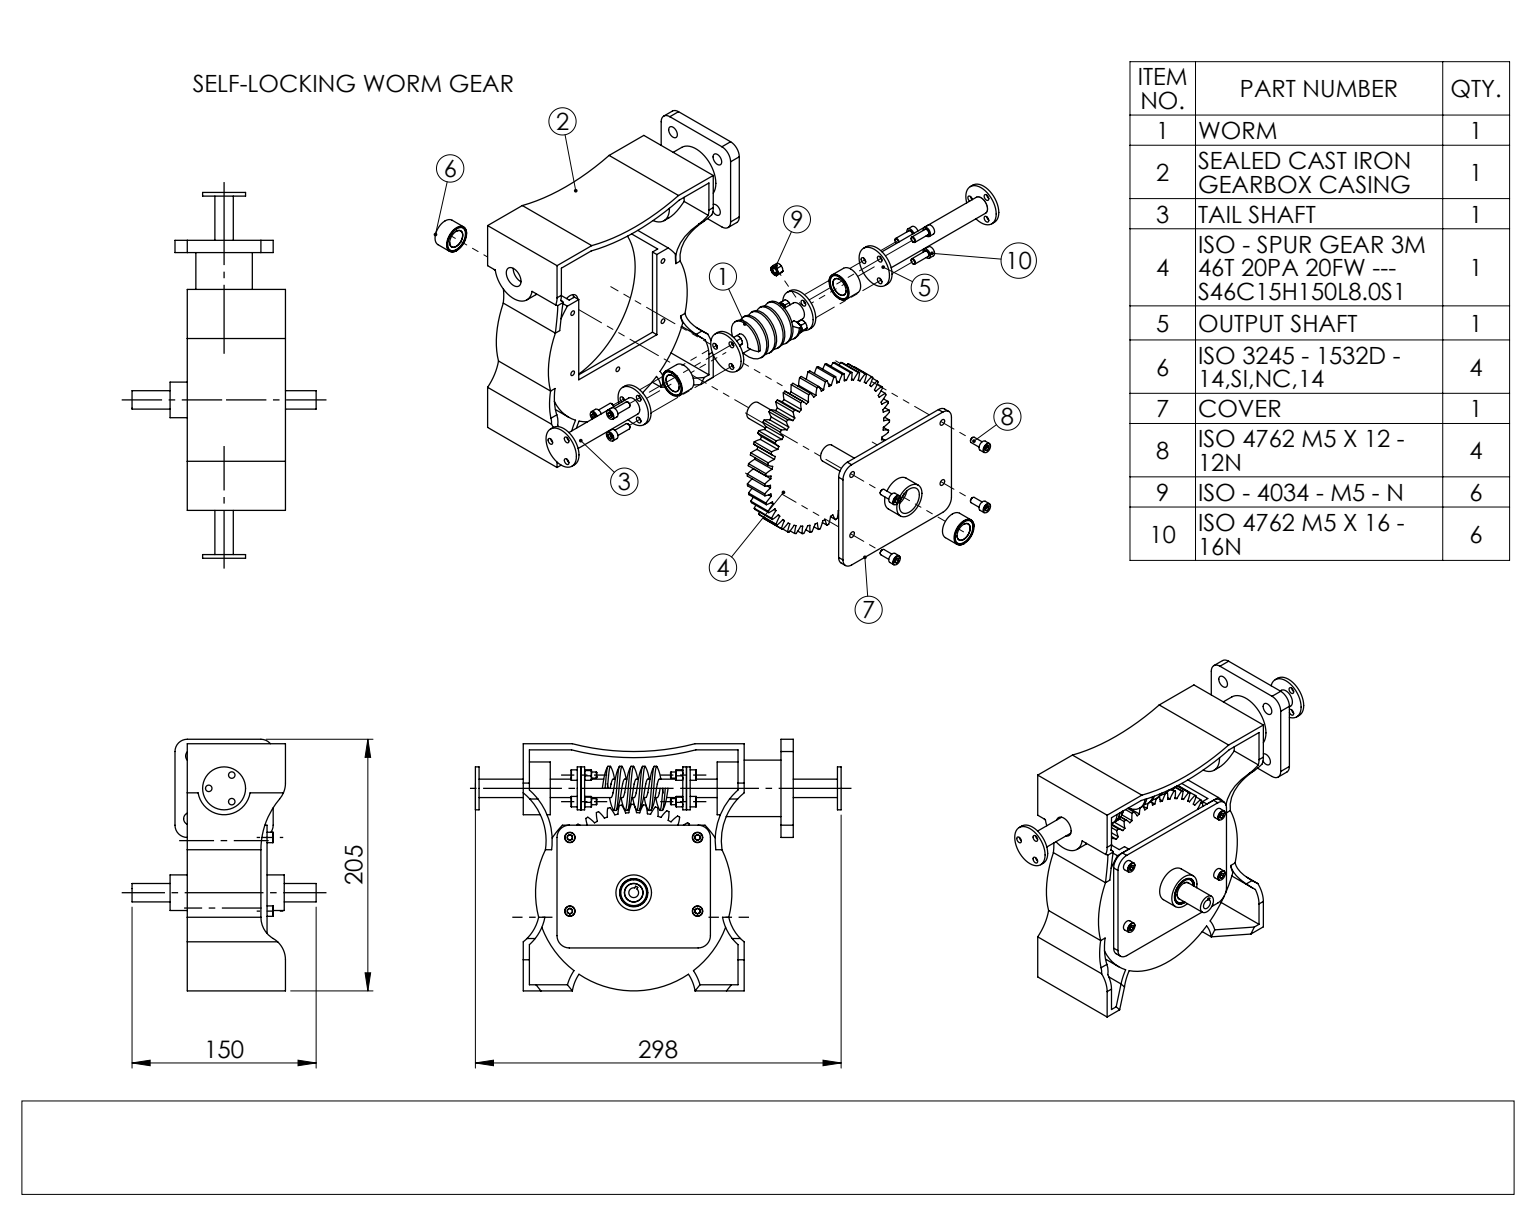
ISO-10303-21;
HEADER;
FILE_DESCRIPTION (('STEP AP214'),
    '1' );
FILE_NAME ('BR-546',
    '2026-10-03T12:29:21',
    ( '' ),
    ( '' ),
    'SwSTEP 2.0',
    'SolidWorks 2026',
    '' );
FILE_SCHEMA (( 'AUTOMOTIVE_DESIGN' ));
ENDSEC;

DATA;
#1 = CARTESIAN_POINT ( 'NONE',  ( 19.99999999999999645, 0.000000000000000000, 0.000000000000000000 ) ) ;
#2 = CARTESIAN_POINT ( 'NONE',  ( -6.358192987158596488, 4.248408730893249441, 12.23479375018031590 ) ) ;
#3 = ADVANCED_FACE ( 'NONE', ( #6649 ), #1884, .F. ) ;
#4 = CARTESIAN_POINT ( 'NONE',  ( 11.17563879758427525, 2.222972768810836719, -0.3496410002868030609 ) ) ;
#5 = ADVANCED_FACE ( 'NONE', ( #12919 ), #11518, .F. ) ;
#6 = DIRECTION ( 'NONE',  ( 0.000000000000000000, 0.000000000000000000, -1.000000000000000000 ) ) ;
#7 = CARTESIAN_POINT ( 'NONE',  ( -30.00000000000000000, -42.57363661491096707, -71.38288848018790134 ) ) ;
#8 = DIRECTION ( 'NONE',  ( 0.000000000000000000, 0.000000000000000000, 1.000000000000000000 ) ) ;
#9 = ORIENTED_EDGE ( 'NONE', *, *, #5715, .F. ) ;
#10 = CYLINDRICAL_SURFACE ( 'NONE', #420, 72.00000000007199219 ) ;
#11 = VERTEX_POINT ( 'NONE', #11628 ) ;
#12 = AXIS2_PLACEMENT_3D ( 'NONE', #6697, #8706, #19835 ) ;
#13 = CARTESIAN_POINT ( 'NONE',  ( 16.62983158437509346, -6.888301784570739272, 14.47261250018031298 ) ) ;
#14 = DIRECTION ( 'NONE',  ( -1.000000000000000000, 0.000000000000000000, 0.000000000000000000 ) ) ;
#15 = ADVANCED_FACE ( 'NONE', ( #19478 ), #14650, .T. ) ;
#16 = ORIENTED_EDGE ( 'NONE', *, *, #12265, .T. ) ;
#17 = CARTESIAN_POINT ( 'NONE',  ( 24.99999999999999645, -39.99999999999999289, 52.00000000000000000 ) ) ;
#18 = EDGE_LOOP ( 'NONE', ( #17253, #7628, #12680, #16637 ) ) ;
#19 = DIRECTION ( 'NONE',  ( -1.000000000000000000, 0.000000000000000000, -0.000000000000000000 ) ) ;
#20 = CARTESIAN_POINT ( 'NONE',  ( 33.05469362121638000, -30.48475803102838100, 72.85691518208254536 ) ) ;
#21 = ORIENTED_EDGE ( 'NONE', *, *, #4326, .F. ) ;
#22 =( GEOMETRIC_REPRESENTATION_CONTEXT ( 3 ) GLOBAL_UNCERTAINTY_ASSIGNED_CONTEXT ( ( #13875 ) ) GLOBAL_UNIT_ASSIGNED_CONTEXT ( ( #2142, #14970, #8601 ) ) REPRESENTATION_CONTEXT ( 'NONE', 'WORKASPACE' ) );
#23 = ORIENTED_EDGE ( 'NONE', *, *, #11876, .F. ) ;
#24 = DIRECTION ( 'NONE',  ( -1.000000000000000000, -0.000000000000000000, 0.000000000000000000 ) ) ;
#25 = CARTESIAN_POINT ( 'NONE',  ( 19.99999999999999645, 0.000000000000000000, 0.000000000000000000 ) ) ;
#26 = EDGE_CURVE ( 'NONE', #19472, #5238, #10237, .T. ) ;
#27 = AXIS2_PLACEMENT_3D ( 'NONE', #16790, #15301, #10014 ) ;
#28 = CARTESIAN_POINT ( 'NONE',  ( -30.00000000000000000, -85.00000000000000000, -1.040949779275250179E-14 ) ) ;
#29 = ORIENTED_EDGE ( 'NONE', *, *, #16424, .T. ) ;
#30 = ADVANCED_FACE ( 'NONE', ( #14609 ), #17902, .T. ) ;
#31 = CARTESIAN_POINT ( 'NONE',  ( -6.358192987158591158, 4.248408730893245000, 5.969893750180312431 ) ) ;
#32 = VECTOR ( 'NONE', #14335, 1000.000000000000000 ) ;
#33 = EDGE_CURVE ( 'NONE', #6658, #4014, #18101, .T. ) ;
#34 = CARTESIAN_POINT ( 'NONE',  ( 6.358192987158596488, -4.248408730893249441, -1.902706249819686279 ) ) ;
#35 = AXIS2_PLACEMENT_3D ( 'NONE', #14775, #17865, #16462 ) ;
#36 = CARTESIAN_POINT ( 'NONE',  ( 0.000000000000000000, 0.000000000000000000, 40.00000000000000000 ) ) ;
#37 = DIRECTION ( 'NONE',  ( 0.000000000000000000, 0.000000000000000000, -1.000000000000000000 ) ) ;
#38 = EDGE_CURVE ( 'NONE', #16141, #4659, #188, .T. ) ;
#39 = ORIENTED_EDGE ( 'NONE', *, *, #4985, .T. ) ;
#40 = DIRECTION ( 'NONE',  ( -0.000000000000000000, -0.000000000000000000, -1.000000000000000000 ) ) ;
#41 = CARTESIAN_POINT ( 'NONE',  ( -6.165580000000000283, 0.000000000000000000, 0.000000000000000000 ) ) ;
#42 = ORIENTED_EDGE ( 'NONE', *, *, #280, .F. ) ;
#43 = PLANE ( 'NONE',  #3162 ) ;
#44 = VERTEX_POINT ( 'NONE', #17992 ) ;
#45 = CARTESIAN_POINT ( 'NONE',  ( 19.99999999999999645, -20.60847369612940128, -61.90898814327737654 ) ) ;
#46 = ORIENTED_EDGE ( 'NONE', *, *, #5820, .T. ) ;
#47 = VECTOR ( 'NONE', #20298, 1000.000000000000000 ) ;
#48 = DIRECTION ( 'NONE',  ( 0.000000000000000000, 0.000000000000000000, -1.000000000000000000 ) ) ;
#49 = EDGE_CURVE ( 'NONE', #12259, #9717, #8442, .T. ) ;
#50 = DIRECTION ( 'NONE',  ( 0.000000000000000000, 0.000000000000000000, -1.000000000000000000 ) ) ;
#51 = CIRCLE ( 'NONE', #6813, 3.199999999999994404 ) ;
#52 = CARTESIAN_POINT ( 'NONE',  ( 14.79893867793684059, 2.943691925285398359, -12.82923933115845649 ) ) ;
#53 = ORIENTED_EDGE ( 'NONE', *, *, #13639, .F. ) ;
#54 = DIRECTION ( 'NONE',  ( 0.000000000000000000, -1.000000000000000000, 0.000000000000000000 ) ) ;
#55 = ADVANCED_FACE ( 'NONE', ( #11330 ), #295, .T. ) ;
#56 = DIRECTION ( 'NONE',  ( 0.000000000000000000, 0.000000000000000000, 1.000000000000000000 ) ) ;
#57 = EDGE_LOOP ( 'NONE', ( #4970, #17934 ) ) ;
#58 = CIRCLE ( 'NONE', #5129, 27.60000000002759890 ) ;
#59 = CARTESIAN_POINT ( 'NONE',  ( 40.00000000000000711, 29.99999999999999289, -120.0000000000000142 ) ) ;
#60 = VECTOR ( 'NONE', #20579, 1000.000000000000000 ) ;
#61 = CARTESIAN_POINT ( 'NONE',  ( -15.25966317163203279, -10.19618095047498052, 17.71245625018031689 ) ) ;
#62 = VECTOR ( 'NONE', #8354, 1000.000000000000000 ) ;
#63 = LINE ( 'NONE', #20325, #13108 ) ;
#64 = DIRECTION ( 'NONE',  ( 0.000000000000000000, 0.000000000000000000, 1.000000000000000000 ) ) ;
#65 = VERTEX_POINT ( 'NONE', #16100 ) ;
#66 = ADVANCED_FACE ( 'NONE', ( #13335 ), #6435, .F. ) ;
#67 = CARTESIAN_POINT ( 'NONE',  ( 0.000000000000000000, 0.000000000000000000, 0.000000000000000000 ) ) ;
#68 =( GEOMETRIC_REPRESENTATION_CONTEXT ( 3 ) GLOBAL_UNCERTAINTY_ASSIGNED_CONTEXT ( ( #15146 ) ) GLOBAL_UNIT_ASSIGNED_CONTEXT ( ( #18068, #7816, #19263 ) ) REPRESENTATION_CONTEXT ( 'NONE', 'WORKASPACE' ) );
#69 = ORIENTED_EDGE ( 'NONE', *, *, #783, .F. ) ;
#70 = CARTESIAN_POINT ( 'NONE',  ( 0.000000000000000000, 38.69327817041775575, 52.53819777490647880 ) ) ;
#71 = DIRECTION ( 'NONE',  ( 0.000000000000000000, 0.000000000000000000, 1.000000000000000000 ) ) ;
#72 = CARTESIAN_POINT ( 'NONE',  ( 1.491842756249030399, 7.499999999820669672, -4.848018749819687834 ) ) ;
#73 = ORIENTED_EDGE ( 'NONE', *, *, #769, .F. ) ;
#74 = DIRECTION ( 'NONE',  ( 0.000000000000000000, 0.4999999999999990008, -0.8660254037844391517 ) ) ;
#75 = AXIS2_PLACEMENT_3D ( 'NONE', #412, #6863, #13354 ) ;
#76 = AXIS2_PLACEMENT_3D ( 'NONE', #4116, #10601, #17063 ) ;
#77 = CARTESIAN_POINT ( 'NONE',  ( -7.500000000000000000, 0.000000000000000000, 126.0000000000000000 ) ) ;
#78 = TOROIDAL_SURFACE ( 'NONE', #2431, 2.700000000000000622, 0.2000000000000000111 ) ;
#79 = APPLICATION_PROTOCOL_DEFINITION ( 'draft international standard', 'automotive_design', 1998, #17252 ) ;
#80 = CARTESIAN_POINT ( 'NONE',  ( 3.580422614997669228, 17.99999999956958874, -7.028168749819693417 ) ) ;
#81 = ORIENTED_EDGE ( 'NONE', *, *, #16157, .T. ) ;
#82 = DIRECTION ( 'NONE',  ( 0.000000000000000000, -0.2697967711570314897, 0.9629172873477973571 ) ) ;
#83 = CARTESIAN_POINT ( 'NONE',  ( -13.67243654778935102, -5.663308646854334327, -4.604354418480926192 ) ) ;
#84 = DIRECTION ( 'NONE',  ( -1.000000000000000000, -0.000000000000000000, -0.000000000000000000 ) ) ;
#85 = VECTOR ( 'NONE', #11262, 1000.000000000000000 ) ;
#86 = ADVANCED_FACE ( 'NONE', ( #9826 ), #1783, .F. ) ;
#87 = ORIENTED_EDGE ( 'NONE', *, *, #13366, .F. ) ;
#88 = EDGE_CURVE ( 'NONE', #14573, #2530, #13132, .T. ) ;
#89 = DIRECTION ( 'NONE',  ( -1.000000000000000000, 0.000000000000000000, 0.000000000000000000 ) ) ;
#90 = DIRECTION ( 'NONE',  ( -0.000000000000000000, -0.000000000000000000, 1.000000000000000000 ) ) ;
#91 = CARTESIAN_POINT ( 'NONE',  ( 150.0000507999999968, 5.400000000000000355, 1.000000000000000000 ) ) ;
#92 = ORIENTED_EDGE ( 'NONE', *, *, #14677, .F. ) ;
#93 = DIRECTION ( 'NONE',  ( -0.000000000000000000, 0.000000000000000000, 1.000000000000000000 ) ) ;
#94 = ORIENTED_EDGE ( 'NONE', *, *, #11160, .T. ) ;
#95 = FACE_OUTER_BOUND ( 'NONE', #12969, .T. ) ;
#96 = CARTESIAN_POINT ( 'NONE',  ( 0.000000000000000000, -3.141410481200616278, -65.17333458706190186 ) ) ;
#97 = B_SPLINE_CURVE_WITH_KNOTS ( 'NONE', 3,
 ( #16276, #17575, #14698, #9503, #6729, #17780 ),
 .UNSPECIFIED., .F., .F.,
 ( 4, 2, 4 ),
 ( 0.002336974151641604130, 0.003500975885716476211, 0.004664977619791348291 ),
 .UNSPECIFIED. ) ;
#98 = ORIENTED_EDGE ( 'NONE', *, *, #9726, .F. ) ;
#99 = AXIS2_PLACEMENT_3D ( 'NONE', #7590, #19041, #10873 ) ;
#100 = VERTEX_POINT ( 'NONE', #5055 ) ;
#101 = CARTESIAN_POINT ( 'NONE',  ( 24.99999999999999645, -39.99999999999999289, -52.00000000000000000 ) ) ;
#102 = FACE_OUTER_BOUND ( 'NONE', #4035, .T. ) ;
#103 = FILL_AREA_STYLE_COLOUR ( '', #1898 ) ;
#104 = LINE ( 'NONE', #16119, #19750 ) ;
#105 = AXIS2_PLACEMENT_3D ( 'NONE', #17790, #10136, #285 ) ;
#106 = AXIS2_PLACEMENT_3D ( 'NONE', #7113, #10104, #5421 ) ;
#107 = CARTESIAN_POINT ( 'NONE',  ( -65.00002539999999840, 3.872983346207417021, 1.000000000000000000 ) ) ;
#108 = CARTESIAN_POINT ( 'NONE',  ( 7.500000000000007994, -9.015933403756345817E-10, 16.06370000018031519 ) ) ;
#109 = EDGE_CURVE ( 'NONE', #12091, #18834, #15657, .T. ) ;
#110 = CARTESIAN_POINT ( 'NONE',  ( -7.902369976724391343, 7.902369978624323110, -3.589484750286802139 ) ) ;
#111 = PLANE ( 'NONE',  #12445 ) ;
#112 = CARTESIAN_POINT ( 'NONE',  ( -44.00000000000000000, -85.00000000000000000, -1.040949779275250179E-14 ) ) ;
#113 = EDGE_LOOP ( 'NONE', ( #18072, #15084 ) ) ;
#114 = CARTESIAN_POINT ( 'NONE',  ( 150.0000507999999968, 0.000000000000000000, 1.000000000000000000 ) ) ;
#115 = CARTESIAN_POINT ( 'NONE',  ( 3.580422614997668340, 17.99999999956958519, 21.24683125018031404 ) ) ;
#116 = DIRECTION ( 'NONE',  ( -1.000000000000000000, -0.000000000000000000, 0.000000000000000000 ) ) ;
#117 = CIRCLE ( 'NONE', #15334, 27.60000000002759890 ) ;
#118 = ORIENTED_EDGE ( 'NONE', *, *, #9973, .F. ) ;
#119 = AXIS2_PLACEMENT_3D ( 'NONE', #12857, #16234, #19212 ) ;
#120 = DIRECTION ( 'NONE',  ( -0.000000000000000000, -0.000000000000000000, 1.000000000000000000 ) ) ;
#121 = ORIENTED_EDGE ( 'NONE', *, *, #380, .T. ) ;
#122 = CARTESIAN_POINT ( 'NONE',  ( 0.000000000000000000, 0.000000000000000000, 5.000000000000000000 ) ) ;
#123 = CARTESIAN_POINT ( 'NONE',  ( 44.16803006078449556, -9.910160788546479083, 83.48928124825249597 ) ) ;
#124 = ORIENTED_EDGE ( 'NONE', *, *, #20626, .F. ) ;
#125 = VERTEX_POINT ( 'NONE', #13749 ) ;
#126 = CARTESIAN_POINT ( 'NONE',  ( -10.00000000000000000, 0.000000000000000000, 0.000000000000000000 ) ) ;
#127 = EDGE_CURVE ( 'NONE', #3649, #15600, #16319, .T. ) ;
#128 = DIRECTION ( 'NONE',  ( 1.000000000000000000, 0.000000000000000000, 0.000000000000000000 ) ) ;
#129 = AXIS2_PLACEMENT_3D ( 'NONE', #17795, #12823, #16096 ) ;
#130 = DIRECTION ( 'NONE',  ( 0.000000000000000000, 0.000000000000000000, -1.000000000000000000 ) ) ;
#131 = AXIS2_PLACEMENT_3D ( 'NONE', #20801, #1327, #6175 ) ;
#132 = EDGE_CURVE ( 'NONE', #3302, #4120, #4083, .T. ) ;
#133 = ORIENTED_EDGE ( 'NONE', *, *, #9590, .F. ) ;
#134 = CIRCLE ( 'NONE', #11980, 27.60000000002760245 ) ;
#135 = CARTESIAN_POINT ( 'NONE',  ( 6.358192988180013216, 4.248408729364577141, 8.915206250180313319 ) ) ;
#136 = DIRECTION ( 'NONE',  ( 0.000000000000000000, 0.000000000000000000, -1.000000000000000000 ) ) ;
#137 = DIRECTION ( 'NONE',  ( 1.000000000000000000, -0.000000000000000000, -0.000000000000000000 ) ) ;
#138 = DIRECTION ( 'NONE',  ( 0.000000000000000000, 0.000000000000000000, -1.000000000000000000 ) ) ;
#139 = ORIENTED_EDGE ( 'NONE', *, *, #678, .F. ) ;
#140 = FACE_OUTER_BOUND ( 'NONE', #16746, .T. ) ;
#141 = VERTEX_POINT ( 'NONE', #18522 ) ;
#142 = CARTESIAN_POINT ( 'NONE',  ( -10.19618095047498052, 15.25966317163203101, 18.16410625018031411 ) ) ;
#143 = CARTESIAN_POINT ( 'NONE',  ( 0.000000000000000000, 0.000000000000000000, 3.469446951953614189E-15 ) ) ;
#144 = ORIENTED_EDGE ( 'NONE', *, *, #13905, .F. ) ;
#145 = CYLINDRICAL_SURFACE ( 'NONE', #1488, 65.24900000006525147 ) ;
#146 = ORIENTED_EDGE ( 'NONE', *, *, #3092, .T. ) ;
#147 = DIRECTION ( 'NONE',  ( 0.000000000000000000, -0.9790840876823206917, -0.2034560130526446298 ) ) ;
#148 = ORIENTED_EDGE ( 'NONE', *, *, #3636, .F. ) ;
#149 = VECTOR ( 'NONE', #9986, 1000.000000000000000 ) ;
#150 = EDGE_CURVE ( 'NONE', #3064, #8629, #754, .T. ) ;
#151 = CIRCLE ( 'NONE', #5555, 10.85999999999999410 ) ;
#152 = EDGE_CURVE ( 'NONE', #4283, #2747, #12613, .T. ) ;
#153 = CARTESIAN_POINT ( 'NONE',  ( 0.000000000000000000, 64.52323195238628273, 6.389157729493382121 ) ) ;
#154 = EDGE_CURVE ( 'NONE', #4126, #11972, #18017, .T. ) ;
#155 = DIRECTION ( 'NONE',  ( -1.000000000000000000, 0.000000000000000000, 0.000000000000000000 ) ) ;
#156 = CARTESIAN_POINT ( 'NONE',  ( 14.79893867722910450, -2.943691928843438443, -21.66517683115846182 ) ) ;
#157 = EDGE_LOOP ( 'NONE', ( #10780, #10369, #19381, #16296 ) ) ;
#158 = DIRECTION ( 'NONE',  ( 0.000000000000000000, 0.000000000000000000, -1.000000000000000000 ) ) ;
#159 = CARTESIAN_POINT ( 'NONE',  ( 6.165579999999999394, 0.000000000000000000, 0.000000000000000000 ) ) ;
#160 = ORIENTED_EDGE ( 'NONE', *, *, #19316, .T. ) ;
#161 = CARTESIAN_POINT ( 'NONE',  ( -21.25952603694473808, -3.390848217253789265, -82.75718265314235111 ) ) ;
#162 = STYLED_ITEM ( 'NONE', ( #18380 ), #10511 ) ;
#163 = DIRECTION ( 'NONE',  ( 0.000000000000000000, 0.000000000000000000, -1.000000000000000000 ) ) ;
#164 = CARTESIAN_POINT ( 'NONE',  ( 21.00000000000000355, 2.516649172247811061E-16, -2.055000000000000160 ) ) ;
#165 = DIRECTION ( 'NONE',  ( -1.000000000000000000, -0.000000000000000000, 0.000000000000000000 ) ) ;
#166 = EDGE_CURVE ( 'NONE', #18682, #10203, #2445, .T. ) ;
#167 = ADVANCED_FACE ( 'NONE', ( #20203 ), #3671, .T. ) ;
#168 = ORIENTED_EDGE ( 'NONE', *, *, #13103, .T. ) ;
#169 = LINE ( 'NONE', #3246, #19204 ) ;
#170 = AXIS2_PLACEMENT_3D ( 'NONE', #9819, #6839, #14708 ) ;
#171 = ORIENTED_EDGE ( 'NONE', *, *, #11662, .T. ) ;
#172 = DIRECTION ( 'NONE',  ( 0.000000000000000000, 0.000000000000000000, -1.000000000000000000 ) ) ;
#173 = DIRECTION ( 'NONE',  ( 0.000000000000000000, 0.000000000000000000, 1.000000000000000000 ) ) ;
#174 = CARTESIAN_POINT ( 'NONE',  ( 3.580422610670019878, -18.00000000043040771, -23.65933124981969016 ) ) ;
#175 = EDGE_CURVE ( 'NONE', #6580, #16499, #15026, .T. ) ;
#176 = ORIENTED_EDGE ( 'NONE', *, *, #6087, .T. ) ;
#177 = CARTESIAN_POINT ( 'NONE',  ( 7.500000000000005329, -1.491842755816077393, -11.91676874991220814 ) ) ;
#178 = AXIS2_PLACEMENT_3D ( 'NONE', #7554, #12660, #3003 ) ;
#179 = CYLINDRICAL_SURFACE ( 'NONE', #11940, 10.52399999999999380 ) ;
#180 = DIRECTION ( 'NONE',  ( -0.1301338387963445198, -0.9914964367057135242, -1.131240564625404877E-16 ) ) ;
#181 =( BOUNDED_SURFACE ( )  B_SPLINE_SURFACE ( 3, 2, ( 
 ( #15242, #3787, #10269, #14938, #18223, #10163, #15145, #724, #8565, #15045, #7180, #2419, #20112, #5588, #10480, #8880, #15353, #840, #7288, #20223, #5698, #2009, #8458, #415, #19801, #11758, #3688, #525, #10588, #12389, #19166, #10700, #7396, #13983, #7499, #17264, #953, #20642, #4431, #1375, #14091, #20319, #7820, #14300, #10899, #18755, #20742, #2956, #17050, #20545, #11002, #18960, #15464, #13872, #17372, #6229, #17163, #6121, #6028, #4541, #2736, #2648, #4336, #12599, #20438, #15878, #5920, #12498, #9205, #19066, #10803, #4224, #17479, #5803, #2537, #18861, #9423, #15665, #1165, #2844, #7613, #9311, #9104, #15774, #12280, #15556, #1276, #12714, #7727, #8994, #1052, #14200, #1778, #4745, #13122, #17792, #9820, #6336, #4647, #14602, #19572, #12822, #16391, #80, #17688, #13019, #3358, #3456, #16196, #16092, #1878, #287, #1683, #5049, #19266, #9516, #3258, #6736, #8232, #9923, #14710, #4852, #20850, #11115, #182, #9728, #1583, #8130, #7931, #8037, #8336, #3157, #6430, #14732, #11212, #16287, #17985, #17586, #6534, #1483, #13219, #12913, #14814, #11512, #19365, #19471, #3054, #6637, #9629, #4953, #15981, #14408, #11323, #11423, #17896, #14513, #5561, #13532, #384, #608, #3977 ),
 ( #813, #3666, #5147, #8432, #501, #10348, #15327, #16915, #13325, #7052, #10457, #11621, #13635, #3757, #8752, #19976, #10138, #16590, #18095, #6840, #19779, #6949, #11829, #5261, #18201, #8536, #20082, #10239, #2079, #15218, #5456, #18293, #11928, #12042, #15017, #18513, #13434, #2395, #19887, #5361, #16701, #3560, #18402, #19667, #2186, #7259, #11730, #16505, #8643, #8852, #15121, #3869, #16813, #700, #2299, #7152, #10037, #14908, #1984, #9079, #2817, #5895, #2616, #7588, #15531, #1025, #5775, #20517, #15431, #8966, #17238, #2927, #2510, #4403, #20194, #10871, #12145, #17342, #4077, #1350, #12367, #15636, #921, #20616, #13847, #7370, #7471, #20291, #17454, #18833, #9397, #4307, #5674, #10777, #2710, #12248, #13953, #15857, #18723, #18614, #4197, #20408, #9287, #13740, #10978, #10675, #1136, #19036, #10557, #7700, #9177, #15748, #14066, #17133, #5999, #17023, #12471, #18935, #1247, #14176, #6092, #12569, #4512, #8205, #12891, #4722, #3337, #16172, #6407, #52, #14684, #11187, #1753, #9596, #19550, #19244, #17659, #16064, #14268, #8110, #7794, #1557, #16368, #7902, #4619, #3127, #8009, #14489, #19145, #17874, #1661, #5030, #11291, #17564, #11491, #17963, #14582, #15950, #3432, #156, #20713 ),
 ( #6506, #9900, #14384, #9797, #17766, #6609, #20929, #20825, #19339, #16266, #4822, #6203, #3232, #12688, #6307, #11091, #9703, #12992, #19445, #3031, #13094, #4926, #9491, #11395, #1450, #12798, #5539, #16678, #10008, #12017, #15197, #10434, #11807, #2272, #10215, #6715, #19644, #2167, #18484, #8411, #18375, #18270, #16784, #14991, #1960, #16568, #11902, #5237, #7127, #18175, #5339, #479, #3845, #2055, #16477, #8731, #18071, #8310, #3642, #10324, #6926, #11707, #8621, #10116, #8510, #14884, #15095, #3536, #361, #3735, #3951, #11596, #13512, #14785, #19955, #264, #5433, #13196, #1856, #13410, #583, #6814, #675, #13298, #19756, #19862, #7033, #5122, #13608, #20055, #1305, #8824, #7748, #9337, #15408, #18696, #19287, #894, #2371, #5650, #4169, #7848, #12843, #14436, #10535, #19097, #1512, #15297, #11138, #14221, #6259, #4570, #7348, #13829, #785, #18593, #16994, #10652, #15801, #2480, #20272, #5750, #17608, #20666, #12226, #12743, #11032, #6148, #9444, #3078, #17107, #9541, #2871, #7963, #12636, #17509, #2983, #7234, #15902, #1400, #19196, #14331, #20776, #4676, #16012, #20881, #6363, #4770, #16894, #13717, #20164, #12125, #4053, #8942, #11237, #13045, #19804, #11351, #8068, #14629, #8156 ),
 ( #19699, #3383, #16418, #12942, #17715, #212, #5180, #19393, #2012, #6669, #3294, #19602, #9954, #10066, #1809, #1707, #8461, #6871, #8261, #11650, #4882, #16123, #9849, #13357, #8369, #16528, #14841, #11455, #6457, #3188, #6767, #16314, #108, #14735, #14537, #6563, #14942, #9758, #19499, #4987, #17823, #1905, #3590, #9657, #13152, #2, #1615, #17923, #418, #18122, #5076, #11542, #16223, #315, #18013, #3480, #13248, #15359, #5486, #7077, #12076, #15047, #12173, #20116, #6975, #7183, #10591, #8571, #958, #528, #18226, #13667, #5700, #18546, #13777, #16624, #10379, #2321, #16844, #7398, #11965, #15244, #2216, #13464, #8674, #7294, #18435, #13556, #15147, #8775, #13876, #632, #5594, #4001, #20227, #10164, #3898, #18323, #15467, #727, #19908, #10483, #2421, #5386, #18639, #16939, #8882, #11855, #5288, #842, #4107, #3790, #17054, #2540, #10273, #8999, #11760, #3692, #2112, #16736, #20004, #15983, #10900, #20745, #13984, #4225, #12499, #1485, #17480, #19168, #2958, #20547, #15560, #20320, #15879, #18963, #10805, #17374, #2650, #17269, #11116, #12392, #1169, #15666, #20443, #11003, #12716, #5805, #9312, #17166, #7936, #7614, #3055, #7821, #14093, #4434, #4650, #9424, #5921, #2847, #1376 ) ),
 .UNSPECIFIED., .F., .F., .F. ) 
 B_SPLINE_SURFACE_WITH_KNOTS ( ( 4, 4 ),
 ( 3, 2, 2, 2, 2, 2, 2, 2, 2, 2, 2, 2, 2, 2, 2, 2, 2, 2, 2, 2, 2, 2, 2, 2, 2, 2, 2, 2, 2, 2, 2, 2, 2, 2, 2, 2, 2, 2, 2, 2, 2, 2, 2, 2, 2, 2, 2, 2, 2, 2, 2, 2, 2, 2, 2, 2, 2, 2, 2, 2, 2, 2, 2, 2, 2, 2, 2, 2, 2, 2, 2, 2, 2, 2, 2, 2, 2, 2, 2, 2, 3 ),
 ( 0.000000000000000000, 1.000000000000000000 ),
 ( 0.000000000000000000, 0.01250000000000000069, 0.02500000000000000139, 0.03749999999999999861, 0.05000000000000000278, 0.06250000000000000000, 0.07499999999999999722, 0.08749999999999999445, 0.1000000000000000056, 0.1125000000000000028, 0.1250000000000000000, 0.1375000000000000111, 0.1499999999999999944, 0.1625000000000000056, 0.1749999999999999889, 0.1875000000000000000, 0.2000000000000000111, 0.2124999999999999944, 0.2250000000000000056, 0.2374999999999999889, 0.2500000000000000000, 0.2625000000000000111, 0.2750000000000000222, 0.2874999999999999778, 0.2999999999999999889, 0.3125000000000000000, 0.3250000000000000111, 0.3375000000000000222, 0.3499999999999999778, 0.3624999999999999889, 0.3750000000000000000, 0.3875000000000000111, 0.4000000000000000222, 0.4124999999999999778, 0.4249999999999999889, 0.4375000000000000000, 0.4500000000000000111, 0.4625000000000000222, 0.4749999999999999778, 0.4874999999999999889, 0.5000000000000000000, 0.5124999999999999556, 0.5250000000000000222, 0.5374999999999999778, 0.5500000000000000444, 0.5625000000000000000, 0.5749999999999999556, 0.5875000000000000222, 0.5999999999999999778, 0.6125000000000000444, 0.6250000000000000000, 0.6374999999999999556, 0.6500000000000000222, 0.6624999999999999778, 0.6750000000000000444, 0.6875000000000000000, 0.6999999999999999556, 0.7125000000000000222, 0.7249999999999999778, 0.7375000000000000444, 0.7500000000000000000, 0.7624999999999999556, 0.7750000000000000222, 0.7874999999999999778, 0.8000000000000000444, 0.8125000000000000000, 0.8249999999999999556, 0.8375000000000000222, 0.8499999999999999778, 0.8625000000000000444, 0.8750000000000000000, 0.8874999999999999556, 0.9000000000000000222, 0.9124999999999999778, 0.9250000000000000444, 0.9375000000000000000, 0.9499999999999999556, 0.9625000000000000222, 0.9749999999999999778, 0.9875000000000000444, 1.000000000000000000 ),
 .UNSPECIFIED. ) 
 GEOMETRIC_REPRESENTATION_ITEM ( )  RATIONAL_B_SPLINE_SURFACE ( (
 ( 1.000000000000000000, 0.9807852804032304306, 1.000000000000000000, 0.9807852804032304306, 1.000000000000000000, 0.9807852804032304306, 1.000000000000000000, 0.9807852804032304306, 1.000000000000000000, 0.9807852804032304306, 1.000000000000000000, 0.9807852804032304306, 1.000000000000000000, 0.9807852804032304306, 1.000000000000000000, 0.9807852804032304306, 1.000000000000000000, 0.9807852804032304306, 1.000000000000000000, 0.9807852804032304306, 1.000000000000000000, 0.9807852804032304306, 1.000000000000000000, 0.9807852804032304306, 1.000000000000000000, 0.9807852804032304306, 1.000000000000000000, 0.9807852804032304306, 1.000000000000000000, 0.9807852804032304306, 1.000000000000000000, 0.9807852804032304306, 1.000000000000000000, 0.9807852804032304306, 1.000000000000000000, 0.9807852804032304306, 1.000000000000000000, 0.9807852804032304306, 1.000000000000000000, 0.9807852804032304306, 1.000000000000000000, 0.9807852804032304306, 1.000000000000000000, 0.9807852804032304306, 1.000000000000000000, 0.9807852804032304306, 1.000000000000000000, 0.9807852804032304306, 1.000000000000000000, 0.9807852804032304306, 1.000000000000000000, 0.9807852804032304306, 1.000000000000000000, 0.9807852804032304306, 1.000000000000000000, 0.9807852804032304306, 1.000000000000000000, 0.9807852804032304306, 1.000000000000000000, 0.9807852804032304306, 1.000000000000000000, 0.9807852804032304306, 1.000000000000000000, 0.9807852804032304306, 1.000000000000000000, 0.9807852804032304306, 1.000000000000000000, 0.9807852804032304306, 1.000000000000000000, 0.9807852804032304306, 1.000000000000000000, 0.9807852804032304306, 1.000000000000000000, 0.9807852804032304306, 1.000000000000000000, 0.9807852804032304306, 1.000000000000000000, 0.9807852804032304306, 1.000000000000000000, 0.9807852804032304306, 1.000000000000000000, 0.9807852804032304306, 1.000000000000000000, 0.9807852804032304306, 1.000000000000000000, 0.9807852804032304306, 1.000000000000000000, 0.9807852804032304306, 1.000000000000000000, 0.9807852804032304306, 1.000000000000000000, 0.9807852804032304306, 1.000000000000000000, 0.9807852804032304306, 1.000000000000000000, 0.9807852804032304306, 1.000000000000000000, 0.9807852804032304306, 1.000000000000000000, 0.9807852804032304306, 1.000000000000000000, 0.9807852804032304306, 1.000000000000000000, 0.9807852804032304306, 1.000000000000000000, 0.9807852804032304306, 1.000000000000000000, 0.9807852804032304306, 1.000000000000000000, 0.9807852804032304306, 1.000000000000000000, 0.9807852804032304306, 1.000000000000000000, 0.9807852804032304306, 1.000000000000000000, 0.9807852804032304306, 1.000000000000000000, 0.9807852804032304306, 1.000000000000000000, 0.9807852804032304306, 1.000000000000000000, 0.9807852804032304306, 1.000000000000000000, 0.9807852804032304306, 1.000000000000000000, 0.9807852804032304306, 1.000000000000000000, 0.9807852804032304306, 1.000000000000000000, 0.9807852804032304306, 1.000000000000000000, 0.9807852804032304306, 1.000000000000000000, 0.9807852804032304306, 1.000000000000000000, 0.9807852804032304306, 1.000000000000000000, 0.9807852804032304306, 1.000000000000000000, 0.9807852804032304306, 1.000000000000000000, 0.9807852804032304306, 1.000000000000000000, 0.9807852804032304306, 1.000000000000000000, 0.9807852804032304306, 1.000000000000000000, 0.9807852804032304306, 1.000000000000000000, 0.9807852804032304306, 1.000000000000000000, 0.9807852804032304306, 1.000000000000000000, 0.9807852804032304306, 1.000000000000000000, 0.9807852804032304306, 1.000000000000000000, 0.9807852804032304306, 1.000000000000000000, 0.9807852804032304306, 1.000000000000000000),
 ( 0.9659702800374152520, 0.9474094319676833464, 0.9659702800374152520, 0.9474094319676833464, 0.9659702800374152520, 0.9474094319676833464, 0.9659702800374152520, 0.9474094319676833464, 0.9659702800374152520, 0.9474094319676833464, 0.9659702800374152520, 0.9474094319676833464, 0.9659702800374152520, 0.9474094319676833464, 0.9659702800374152520, 0.9474094319676833464, 0.9659702800374152520, 0.9474094319676833464, 0.9659702800374152520, 0.9474094319676833464, 0.9659702800374152520, 0.9474094319676833464, 0.9659702800374152520, 0.9474094319676833464, 0.9659702800374152520, 0.9474094319676833464, 0.9659702800374152520, 0.9474094319676833464, 0.9659702800374152520, 0.9474094319676833464, 0.9659702800374152520, 0.9474094319676833464, 0.9659702800374152520, 0.9474094319676833464, 0.9659702800374152520, 0.9474094319676833464, 0.9659702800374152520, 0.9474094319676833464, 0.9659702800374152520, 0.9474094319676833464, 0.9659702800374152520, 0.9474094319676833464, 0.9659702800374152520, 0.9474094319676833464, 0.9659702800374152520, 0.9474094319676833464, 0.9659702800374152520, 0.9474094319676833464, 0.9659702800374152520, 0.9474094319676833464, 0.9659702800374152520, 0.9474094319676833464, 0.9659702800374152520, 0.9474094319676833464, 0.9659702800374152520, 0.9474094319676833464, 0.9659702800374152520, 0.9474094319676833464, 0.9659702800374152520, 0.9474094319676833464, 0.9659702800374152520, 0.9474094319676833464, 0.9659702800374152520, 0.9474094319676833464, 0.9659702800374152520, 0.9474094319676833464, 0.9659702800374152520, 0.9474094319676833464, 0.9659702800374152520, 0.9474094319676833464, 0.9659702800374152520, 0.9474094319676833464, 0.9659702800374152520, 0.9474094319676833464, 0.9659702800374152520, 0.9474094319676833464, 0.9659702800374152520, 0.9474094319676833464, 0.9659702800374152520, 0.9474094319676833464, 0.9659702800374152520, 0.9474094319676833464, 0.9659702800374152520, 0.9474094319676833464, 0.9659702800374152520, 0.9474094319676833464, 0.9659702800374152520, 0.9474094319676833464, 0.9659702800374152520, 0.9474094319676833464, 0.9659702800374152520, 0.9474094319676833464, 0.9659702800374152520, 0.9474094319676833464, 0.9659702800374152520, 0.9474094319676833464, 0.9659702800374152520, 0.9474094319676833464, 0.9659702800374152520, 0.9474094319676833464, 0.9659702800374152520, 0.9474094319676833464, 0.9659702800374152520, 0.9474094319676833464, 0.9659702800374152520, 0.9474094319676833464, 0.9659702800374152520, 0.9474094319676833464, 0.9659702800374152520, 0.9474094319676833464, 0.9659702800374152520, 0.9474094319676833464, 0.9659702800374152520, 0.9474094319676833464, 0.9659702800374152520, 0.9474094319676833464, 0.9659702800374152520, 0.9474094319676833464, 0.9659702800374152520, 0.9474094319676833464, 0.9659702800374152520, 0.9474094319676833464, 0.9659702800374152520, 0.9474094319676833464, 0.9659702800374152520, 0.9474094319676833464, 0.9659702800374152520, 0.9474094319676833464, 0.9659702800374152520, 0.9474094319676833464, 0.9659702800374152520, 0.9474094319676833464, 0.9659702800374152520, 0.9474094319676833464, 0.9659702800374152520, 0.9474094319676833464, 0.9659702800374152520, 0.9474094319676833464, 0.9659702800374152520, 0.9474094319676833464, 0.9659702800374152520, 0.9474094319676833464, 0.9659702800374152520, 0.9474094319676833464, 0.9659702800374152520, 0.9474094319676833464, 0.9659702800374152520, 0.9474094319676833464, 0.9659702800374152520, 0.9474094319676833464, 0.9659702800374152520, 0.9474094319676833464, 0.9659702800374152520, 0.9474094319676833464, 0.9659702800374152520, 0.9474094319676833464, 0.9659702800374152520, 0.9474094319676833464, 0.9659702800374152520, 0.9474094319676833464, 0.9659702800374152520),
 ( 0.9659702800374152520, 0.9474094319676833464, 0.9659702800374152520, 0.9474094319676833464, 0.9659702800374152520, 0.9474094319676833464, 0.9659702800374152520, 0.9474094319676833464, 0.9659702800374152520, 0.9474094319676833464, 0.9659702800374152520, 0.9474094319676833464, 0.9659702800374152520, 0.9474094319676833464, 0.9659702800374152520, 0.9474094319676833464, 0.9659702800374152520, 0.9474094319676833464, 0.9659702800374152520, 0.9474094319676833464, 0.9659702800374152520, 0.9474094319676833464, 0.9659702800374152520, 0.9474094319676833464, 0.9659702800374152520, 0.9474094319676833464, 0.9659702800374152520, 0.9474094319676833464, 0.9659702800374152520, 0.9474094319676833464, 0.9659702800374152520, 0.9474094319676833464, 0.9659702800374152520, 0.9474094319676833464, 0.9659702800374152520, 0.9474094319676833464, 0.9659702800374152520, 0.9474094319676833464, 0.9659702800374152520, 0.9474094319676833464, 0.9659702800374152520, 0.9474094319676833464, 0.9659702800374152520, 0.9474094319676833464, 0.9659702800374152520, 0.9474094319676833464, 0.9659702800374152520, 0.9474094319676833464, 0.9659702800374152520, 0.9474094319676833464, 0.9659702800374152520, 0.9474094319676833464, 0.9659702800374152520, 0.9474094319676833464, 0.9659702800374152520, 0.9474094319676833464, 0.9659702800374152520, 0.9474094319676833464, 0.9659702800374152520, 0.9474094319676833464, 0.9659702800374152520, 0.9474094319676833464, 0.9659702800374152520, 0.9474094319676833464, 0.9659702800374152520, 0.9474094319676833464, 0.9659702800374152520, 0.9474094319676833464, 0.9659702800374152520, 0.9474094319676833464, 0.9659702800374152520, 0.9474094319676833464, 0.9659702800374152520, 0.9474094319676833464, 0.9659702800374152520, 0.9474094319676833464, 0.9659702800374152520, 0.9474094319676833464, 0.9659702800374152520, 0.9474094319676833464, 0.9659702800374152520, 0.9474094319676833464, 0.9659702800374152520, 0.9474094319676833464, 0.9659702800374152520, 0.9474094319676833464, 0.9659702800374152520, 0.9474094319676833464, 0.9659702800374152520, 0.9474094319676833464, 0.9659702800374152520, 0.9474094319676833464, 0.9659702800374152520, 0.9474094319676833464, 0.9659702800374152520, 0.9474094319676833464, 0.9659702800374152520, 0.9474094319676833464, 0.9659702800374152520, 0.9474094319676833464, 0.9659702800374152520, 0.9474094319676833464, 0.9659702800374152520, 0.9474094319676833464, 0.9659702800374152520, 0.9474094319676833464, 0.9659702800374152520, 0.9474094319676833464, 0.9659702800374152520, 0.9474094319676833464, 0.9659702800374152520, 0.9474094319676833464, 0.9659702800374152520, 0.9474094319676833464, 0.9659702800374152520, 0.9474094319676833464, 0.9659702800374152520, 0.9474094319676833464, 0.9659702800374152520, 0.9474094319676833464, 0.9659702800374152520, 0.9474094319676833464, 0.9659702800374152520, 0.9474094319676833464, 0.9659702800374152520, 0.9474094319676833464, 0.9659702800374152520, 0.9474094319676833464, 0.9659702800374152520, 0.9474094319676833464, 0.9659702800374152520, 0.9474094319676833464, 0.9659702800374152520, 0.9474094319676833464, 0.9659702800374152520, 0.9474094319676833464, 0.9659702800374152520, 0.9474094319676833464, 0.9659702800374152520, 0.9474094319676833464, 0.9659702800374152520, 0.9474094319676833464, 0.9659702800374152520, 0.9474094319676833464, 0.9659702800374152520, 0.9474094319676833464, 0.9659702800374152520, 0.9474094319676833464, 0.9659702800374152520, 0.9474094319676833464, 0.9659702800374152520, 0.9474094319676833464, 0.9659702800374152520, 0.9474094319676833464, 0.9659702800374152520, 0.9474094319676833464, 0.9659702800374152520, 0.9474094319676833464, 0.9659702800374152520, 0.9474094319676833464, 0.9659702800374152520),
 ( 1.000000000000000000, 0.9807852804032304306, 1.000000000000000000, 0.9807852804032304306, 1.000000000000000000, 0.9807852804032304306, 1.000000000000000000, 0.9807852804032304306, 1.000000000000000000, 0.9807852804032304306, 1.000000000000000000, 0.9807852804032304306, 1.000000000000000000, 0.9807852804032304306, 1.000000000000000000, 0.9807852804032304306, 1.000000000000000000, 0.9807852804032304306, 1.000000000000000000, 0.9807852804032304306, 1.000000000000000000, 0.9807852804032304306, 1.000000000000000000, 0.9807852804032304306, 1.000000000000000000, 0.9807852804032304306, 1.000000000000000000, 0.9807852804032304306, 1.000000000000000000, 0.9807852804032304306, 1.000000000000000000, 0.9807852804032304306, 1.000000000000000000, 0.9807852804032304306, 1.000000000000000000, 0.9807852804032304306, 1.000000000000000000, 0.9807852804032304306, 1.000000000000000000, 0.9807852804032304306, 1.000000000000000000, 0.9807852804032304306, 1.000000000000000000, 0.9807852804032304306, 1.000000000000000000, 0.9807852804032304306, 1.000000000000000000, 0.9807852804032304306, 1.000000000000000000, 0.9807852804032304306, 1.000000000000000000, 0.9807852804032304306, 1.000000000000000000, 0.9807852804032304306, 1.000000000000000000, 0.9807852804032304306, 1.000000000000000000, 0.9807852804032304306, 1.000000000000000000, 0.9807852804032304306, 1.000000000000000000, 0.9807852804032304306, 1.000000000000000000, 0.9807852804032304306, 1.000000000000000000, 0.9807852804032304306, 1.000000000000000000, 0.9807852804032304306, 1.000000000000000000, 0.9807852804032304306, 1.000000000000000000, 0.9807852804032304306, 1.000000000000000000, 0.9807852804032304306, 1.000000000000000000, 0.9807852804032304306, 1.000000000000000000, 0.9807852804032304306, 1.000000000000000000, 0.9807852804032304306, 1.000000000000000000, 0.9807852804032304306, 1.000000000000000000, 0.9807852804032304306, 1.000000000000000000, 0.9807852804032304306, 1.000000000000000000, 0.9807852804032304306, 1.000000000000000000, 0.9807852804032304306, 1.000000000000000000, 0.9807852804032304306, 1.000000000000000000, 0.9807852804032304306, 1.000000000000000000, 0.9807852804032304306, 1.000000000000000000, 0.9807852804032304306, 1.000000000000000000, 0.9807852804032304306, 1.000000000000000000, 0.9807852804032304306, 1.000000000000000000, 0.9807852804032304306, 1.000000000000000000, 0.9807852804032304306, 1.000000000000000000, 0.9807852804032304306, 1.000000000000000000, 0.9807852804032304306, 1.000000000000000000, 0.9807852804032304306, 1.000000000000000000, 0.9807852804032304306, 1.000000000000000000, 0.9807852804032304306, 1.000000000000000000, 0.9807852804032304306, 1.000000000000000000, 0.9807852804032304306, 1.000000000000000000, 0.9807852804032304306, 1.000000000000000000, 0.9807852804032304306, 1.000000000000000000, 0.9807852804032304306, 1.000000000000000000, 0.9807852804032304306, 1.000000000000000000, 0.9807852804032304306, 1.000000000000000000, 0.9807852804032304306, 1.000000000000000000, 0.9807852804032304306, 1.000000000000000000, 0.9807852804032304306, 1.000000000000000000, 0.9807852804032304306, 1.000000000000000000, 0.9807852804032304306, 1.000000000000000000, 0.9807852804032304306, 1.000000000000000000, 0.9807852804032304306, 1.000000000000000000, 0.9807852804032304306, 1.000000000000000000, 0.9807852804032304306, 1.000000000000000000, 0.9807852804032304306, 1.000000000000000000, 0.9807852804032304306, 1.000000000000000000, 0.9807852804032304306, 1.000000000000000000, 0.9807852804032304306, 1.000000000000000000, 0.9807852804032304306, 1.000000000000000000, 0.9807852804032304306, 1.000000000000000000) ) ) 
 REPRESENTATION_ITEM ( '' )  SURFACE ( )  );
#182 = CARTESIAN_POINT ( 'NONE',  ( 12.72792205982779912, -12.72792206288791483, -13.21332499981969022 ) ) ;
#183 = ORIENTED_EDGE ( 'NONE', *, *, #18142, .F. ) ;
#184 = FACE_OUTER_BOUND ( 'NONE', #4764, .T. ) ;
#185 = DIRECTION ( 'NONE',  ( 1.000000000000000000, 0.000000000000000000, 0.000000000000000000 ) ) ;
#186 = CARTESIAN_POINT ( 'NONE',  ( 1.779017513685135741E-09, 14.79893867758296544, -1.659041918480926858 ) ) ;
#187 = AXIS2_PLACEMENT_3D ( 'NONE', #9461, #14239, #12440 ) ;
#188 = LINE ( 'NONE', #16294, #20046 ) ;
#189 = APPLICATION_CONTEXT ( 'automotive_design' ) ;
#190 = CIRCLE ( 'NONE', #11381, 7.500000000000000000 ) ;
#191 = ORIENTED_EDGE ( 'NONE', *, *, #7409, .T. ) ;
#192 = DIRECTION ( 'NONE',  ( -1.000000000000000000, 0.000000000000000000, 0.000000000000000000 ) ) ;
#193 = PLANE ( 'NONE',  #2937 ) ;
#194 = DIRECTION ( 'NONE',  ( 1.000000000000000000, 0.000000000000000000, 0.000000000000000000 ) ) ;
#195 = ORIENTED_EDGE ( 'NONE', *, *, #17248, .F. ) ;
#196 = DIRECTION ( 'NONE',  ( -1.000000000000000000, -0.000000000000000000, -0.000000000000000000 ) ) ;
#197 = VERTEX_POINT ( 'NONE', #8975 ) ;
#198 = CARTESIAN_POINT ( 'NONE',  ( 0.000000000000000000, 0.000000000000000000, 0.000000000000000000 ) ) ;
#199 = DIRECTION ( 'NONE',  ( 0.000000000000000000, 0.000000000000000000, 1.000000000000000000 ) ) ;
#200 = VERTEX_POINT ( 'NONE', #10355 ) ;
#201 = ORIENTED_EDGE ( 'NONE', *, *, #18377, .T. ) ;
#202 = DIRECTION ( 'NONE',  ( 0.000000000000000000, 0.8660254037844380415, -0.5000000000000012212 ) ) ;
#203 = AXIS2_PLACEMENT_3D ( 'NONE', #3155, #20849, #4430 ) ;
#204 = CIRCLE ( 'NONE', #9346, 4.000000000000000888 ) ;
#205 = DIRECTION ( 'NONE',  ( 0.000000000000000000, 0.000000000000000000, -1.000000000000000000 ) ) ;
#206 =( NAMED_UNIT ( * ) SI_UNIT ( $, .STERADIAN. ) SOLID_ANGLE_UNIT ( ) );
#207 = DIRECTION ( 'NONE',  ( 0.000000000000000000, 0.000000000000000000, 1.000000000000000000 ) ) ;
#208 = VECTOR ( 'NONE', #12134, 1000.000000000000000 ) ;
#209 = VECTOR ( 'NONE', #12697, 1000.000000000000114 ) ;
#210 = EDGE_CURVE ( 'NONE', #9883, #2104, #5368, .T. ) ;
#211 = DIRECTION ( 'NONE',  ( 1.000000000000000000, 0.000000000000000000, 0.000000000000000000 ) ) ;
#212 = CARTESIAN_POINT ( 'NONE',  ( 4.248408730893249441, 6.358192987158595599, 24.01604375018031945 ) ) ;
#213 = CARTESIAN_POINT ( 'NONE',  ( -2.222972771497743416, -11.17563879704981566, 12.02067149971319893 ) ) ;
#214 = CIRCLE ( 'NONE', #10382, 27.60000000002759535 ) ;
#215 = DIRECTION ( 'NONE',  ( 1.000000000000000000, 0.000000000000000000, 0.000000000000000000 ) ) ;
#216 = LINE ( 'NONE', #11142, #13413 ) ;
#217 = VECTOR ( 'NONE', #18691, 1000.000000000000000 ) ;
#218 = EDGE_LOOP ( 'NONE', ( #4264, #16407, #7924, #14163 ) ) ;
#219 = CYLINDRICAL_SURFACE ( 'NONE', #12266, 2.649999999999992806 ) ;
#220 = VECTOR ( 'NONE', #17502, 1000.000000000000000 ) ;
#221 = CARTESIAN_POINT ( 'NONE',  ( 2.163825119083639534E-09, 18.00000000000000000, 11.52730000018031298 ) ) ;
#222 = CARTESIAN_POINT ( 'NONE',  ( 30.00000000000000000, -99.99999999999998579, -52.00000000000000000 ) ) ;
#223 = ORIENTED_EDGE ( 'NONE', *, *, #11424, .T. ) ;
#224 = DIRECTION ( 'NONE',  ( -1.000000000000000000, -0.000000000000000000, -0.000000000000000000 ) ) ;
#225 = AXIS2_PLACEMENT_3D ( 'NONE', #9690, #19631, #5323 ) ;
#226 = EDGE_LOOP ( 'NONE', ( #12803, #12850, #13208, #16492, #13588 ) ) ;
#227 = AXIS2_PLACEMENT_3D ( 'NONE', #13728, #8834, #15310 ) ;
#228 = CARTESIAN_POINT ( 'NONE',  ( 50.00000000000000000, -110.0000000000000000, -45.00000000000000711 ) ) ;
#229 = CARTESIAN_POINT ( 'NONE',  ( 31.94499812652455617, -34.25508116175669215, 72.04208363913775770 ) ) ;
#230 = MECHANICAL_DESIGN_GEOMETRIC_PRESENTATION_REPRESENTATION (  '', ( #19516 ), #11670 ) ;
#231 = VERTEX_POINT ( 'NONE', #15440 ) ;
#232 = VERTEX_POINT ( 'NONE', #20093 ) ;
#233 = DIRECTION ( 'NONE',  ( 1.000000000000000000, 0.000000000000000000, 0.000000000000000000 ) ) ;
#234 =( LENGTH_UNIT ( ) NAMED_UNIT ( * ) SI_UNIT ( .MILLI., .METRE. ) );
#235 = FACE_OUTER_BOUND ( 'NONE', #1622, .T. ) ;
#236 = ADVANCED_FACE ( 'NONE', ( #17031 ), #2519, .F. ) ;
#237 = CONICAL_SURFACE ( 'NONE', #4643, 2.500000000000002220, 0.9599310885968777018 ) ;
#238 = CARTESIAN_POINT ( 'NONE',  ( -52.49999999999999289, -30.00000000000000000, 0.000000000000000000 ) ) ;
#239 = ORIENTED_EDGE ( 'NONE', *, *, #11369, .T. ) ;
#240 = AXIS2_PLACEMENT_3D ( 'NONE', #14283, #9409, #6012 ) ;
#241 = CARTESIAN_POINT ( 'NONE',  ( -7.499999999820661678, 1.491842756249031288, 14.80583125018031154 ) ) ;
#242 = CIRCLE ( 'NONE', #15142, 72.00000000007199219 ) ;
#243 = CARTESIAN_POINT ( 'NONE',  ( 31.48472450438898207, -112.5746437239468776, -80.05721278606669955 ) ) ;
#244 = DIRECTION ( 'NONE',  ( 1.000000000000000000, 0.000000000000000000, 0.000000000000000000 ) ) ;
#245 = CARTESIAN_POINT ( 'NONE',  ( 19.99999999999999645, 0.000000000000000000, 0.000000000000000000 ) ) ;
#246 = DIRECTION ( 'NONE',  ( -1.000000000000000000, 0.000000000000000000, 0.000000000000000000 ) ) ;
#247 = ADVANCED_FACE ( 'NONE', ( #7269 ), #15224, .T. ) ;
#248 = ORIENTED_EDGE ( 'NONE', *, *, #5986, .F. ) ;
#249 = DIRECTION ( 'NONE',  ( -0.000000000000000000, -0.000000000000000000, 1.000000000000000000 ) ) ;
#250 = ORIENTED_EDGE ( 'NONE', *, *, #12738, .T. ) ;
#251 = LINE ( 'NONE', #19844, #9700 ) ;
#252 = DIRECTION ( 'NONE',  ( -1.000000000000000000, -0.000000000000000000, -0.000000000000000000 ) ) ;
#253 = VECTOR ( 'NONE', #13446, 1000.000000000000000 ) ;
#254 = VERTEX_POINT ( 'NONE', #932 ) ;
#255 = DIRECTION ( 'NONE',  ( -1.000000000000000000, -0.000000000000000000, -0.000000000000000000 ) ) ;
#256 = ORIENTED_EDGE ( 'NONE', *, *, #14101, .F. ) ;
#257 = LINE ( 'NONE', #14576, #12551 ) ;
#258 = CIRCLE ( 'NONE', #12801, 17.50000000000000355 ) ;
#259 = EDGE_LOOP ( 'NONE', ( #20380, #378, #6522, #9090 ) ) ;
#260 = VECTOR ( 'NONE', #15777, 1000.000000000000000 ) ;
#261 = LINE ( 'NONE', #14579, #14811 ) ;
#262 = CARTESIAN_POINT ( 'NONE',  ( 0.000000000000000000, 0.000000000000000000, 84.99999999999998579 ) ) ;
#263 = AXIS2_PLACEMENT_3D ( 'NONE', #7440, #2362, #13920 ) ;
#264 = CARTESIAN_POINT ( 'NONE',  ( -6.330490856366295382, 9.474249098604511587, 3.827766000647429667 ) ) ;
#265 = ORIENTED_EDGE ( 'NONE', *, *, #15414, .F. ) ;
#266 = CARTESIAN_POINT ( 'NONE',  ( 5.000000000000004441, 5.204748896376250699E-16, -4.250000000000000000 ) ) ;
#267 = ADVANCED_FACE ( 'NONE', ( #2088, #12152 ), #10146, .T. ) ;
#268 = CIRCLE ( 'NONE', #17552, 27.60000000002759890 ) ;
#269 = DIRECTION ( 'NONE',  ( -1.000000000000000000, 0.000000000000000000, 0.000000000000000000 ) ) ;
#270 = EDGE_LOOP ( 'NONE', ( #12954, #8026, #4477, #571 ) ) ;
#271 = DIRECTION ( 'NONE',  ( -0.000000000000000000, -0.000000000000000000, -1.000000000000000000 ) ) ;
#272 = EDGE_CURVE ( 'NONE', #19715, #5449, #20689, .T. ) ;
#273 = VERTEX_POINT ( 'NONE', #11836 ) ;
#274 = EDGE_CURVE ( 'NONE', #4186, #16423, #8543, .T. ) ;
#275 = CARTESIAN_POINT ( 'NONE',  ( 10.19618095047497874, -15.25966317163203279, 15.35620625018031404 ) ) ;
#276 = DIRECTION ( 'NONE',  ( 0.000000000000000000, 0.000000000000000000, 1.000000000000000000 ) ) ;
#277 = DIRECTION ( 'NONE',  ( 0.000000000000000000, 0.000000000000000000, 1.000000000000000000 ) ) ;
#278 = EDGE_LOOP ( 'NONE', ( #9863, #20923 ) ) ;
#279 = FACE_BOUND ( 'NONE', #8489, .T. ) ;
#280 = EDGE_CURVE ( 'NONE', #8357, #19645, #2082, .T. ) ;
#281 = VERTEX_POINT ( 'NONE', #13962 ) ;
#282 = DIRECTION ( 'NONE',  ( -1.000000000000000000, -0.000000000000000000, -0.000000000000000000 ) ) ;
#283 = ORIENTED_EDGE ( 'NONE', *, *, #9192, .T. ) ;
#284 = CARTESIAN_POINT ( 'NONE',  ( 0.000000000000000000, 0.000000000000000000, 0.000000000000000000 ) ) ;
#285 = DIRECTION ( 'NONE',  ( 0.000000000000000000, 1.000000000000000000, 0.000000000000000000 ) ) ;
#286 = PRODUCT_CONTEXT ( 'NONE', #3554, 'mechanical' ) ;
#287 = CARTESIAN_POINT ( 'NONE',  ( -17.99999999956958874, 3.580422614997675002, -9.384418749819689154 ) ) ;
#288 = EDGE_CURVE ( 'NONE', #12045, #14031, #12238, .T. ) ;
#289 = ORIENTED_EDGE ( 'NONE', *, *, #11135, .F. ) ;
#290 = CARTESIAN_POINT ( 'NONE',  ( 1.491842756249029289, 7.499999999820664343, 7.737081250180308345 ) ) ;
#291 = CYLINDRICAL_SURFACE ( 'NONE', #18893, 65.24900000006525147 ) ;
#292 = EDGE_CURVE ( 'NONE', #16213, #10742, #11099, .T. ) ;
#293 = CARTESIAN_POINT ( 'NONE',  ( 14.79893867793683349, 2.943691925285396582, 0.4026768315190735747 ) ) ;
#294 = EDGE_CURVE ( 'NONE', #19785, #7832, #9854, .T. ) ;
#295 = CYLINDRICAL_SURFACE ( 'NONE', #11260, 80.00000000000000000 ) ;
#296 = EDGE_CURVE ( 'NONE', #10832, #9434, #9184, .T. ) ;
#297 = VERTEX_POINT ( 'NONE', #18840 ) ;
#298 = DIRECTION ( 'NONE',  ( -1.000000000000000000, -0.000000000000000000, -0.000000000000000000 ) ) ;
#299 = CARTESIAN_POINT ( 'NONE',  ( 0.000000000000000000, 0.000000000000000000, 46.00000000000000711 ) ) ;
#300 = CARTESIAN_POINT ( 'NONE',  ( 4.248408730893246776, 6.358192987158592047, 17.75114375018031154 ) ) ;
#301 = EDGE_LOOP ( 'NONE', ( #6939, #11151, #11050, #12227 ) ) ;
#302 = FACE_OUTER_BOUND ( 'NONE', #301, .T. ) ;
#303 = ORIENTED_EDGE ( 'NONE', *, *, #14253, .T. ) ;
#304 = FACE_OUTER_BOUND ( 'NONE', #4733, .T. ) ;
#305 = DIRECTION ( 'NONE',  ( -1.000000000000000000, 0.000000000000000000, -0.000000000000000000 ) ) ;
#306 = VERTEX_POINT ( 'NONE', #7710 ) ;
#307 = ORIENTED_EDGE ( 'NONE', *, *, #11823, .T. ) ;
#308 = CARTESIAN_POINT ( 'NONE',  ( 19.99999999999999645, 3.141410481201988070, -65.17333458706183080 ) ) ;
#309 = CARTESIAN_POINT ( 'NONE',  ( -10.00000000000000000, 0.000000000000000000, 0.000000000000000000 ) ) ;
#310 = LINE ( 'NONE', #8363, #85 ) ;
#311 = CARTESIAN_POINT ( 'NONE',  ( 19.99999999999999645, 0.000000000000000000, 0.000000000000000000 ) ) ;
#312 = ADVANCED_FACE ( 'NONE', ( #5902 ), #17141, .T. ) ;
#313 = UNCERTAINTY_MEASURE_WITH_UNIT (LENGTH_MEASURE( 1.000000000000000082E-05 ), #19598, 'distance_accuracy_value', 'NONE');
#314 = DIRECTION ( 'NONE',  ( -0.000000000000000000, -0.000000000000000000, 1.000000000000000000 ) ) ;
#315 = CARTESIAN_POINT ( 'NONE',  ( -4.248408730893249441, -6.358192987158595599, 9.878543750180314831 ) ) ;
#316 = APPLICATION_CONTEXT ( 'automotive_design' ) ;
#317 = CARTESIAN_POINT ( 'NONE',  ( 10.32494394706615637, -4.276731815070946574, 9.958952749713198216 ) ) ;
#318 = DIRECTION ( 'NONE',  ( 0.000000000000000000, -0.4999999999999993894, 0.8660254037844389297 ) ) ;
#319 = CARTESIAN_POINT ( 'NONE',  ( 2.099999999999999645, 0.000000000000000000, -5.599999999999999645 ) ) ;
#320 = ORIENTED_EDGE ( 'NONE', *, *, #19952, .T. ) ;
#321 = DIRECTION ( 'NONE',  ( -1.000000000000000000, 0.000000000000000000, 0.000000000000000000 ) ) ;
#322 = CARTESIAN_POINT ( 'NONE',  ( 15.25966316918061416, -10.19618095414378622, 14.76714375018031333 ) ) ;
#323 = CARTESIAN_POINT ( 'NONE',  ( 0.000000000000000000, -44.69367065308607323, -56.44887778834792869 ) ) ;
#324 = ORIENTED_EDGE ( 'NONE', *, *, #1202, .T. ) ;
#325 = DIRECTION ( 'NONE',  ( -1.000000000000000000, -0.000000000000000000, 0.000000000000000000 ) ) ;
#326 = AXIS2_PLACEMENT_3D ( 'NONE', #1007, #15102, #2907 ) ;
#327 = ORIENTED_EDGE ( 'NONE', *, *, #8085, .T. ) ;
#328 = LINE ( 'NONE', #4786, #20321 ) ;
#329 = CARTESIAN_POINT ( 'NONE',  ( -31.74999999999995737, 3.061616997868383634E-16, -2.500000000000000444 ) ) ;
#330 = ADVANCED_FACE ( 'NONE', ( #4521 ), #3038, .T. ) ;
#331 = ORIENTED_EDGE ( 'NONE', *, *, #12503, .F. ) ;
#332 = ORIENTED_EDGE ( 'NONE', *, *, #5820, .F. ) ;
#333 = DIRECTION ( 'NONE',  ( -1.000000000000000000, 0.000000000000000000, 0.000000000000000000 ) ) ;
#334 = SURFACE_STYLE_USAGE ( .BOTH. , #6692 ) ;
#335 = CARTESIAN_POINT ( 'NONE',  ( 2.500000000000000000, 2.357898499370433054, -1.951563910473907981E-15 ) ) ;
#336 = DIRECTION ( 'NONE',  ( 1.000000000000000000, 0.000000000000000000, 0.000000000000000000 ) ) ;
#337 = ORIENTED_EDGE ( 'NONE', *, *, #5451, .T. ) ;
#338 = CARTESIAN_POINT ( 'NONE',  ( 7.500000000179339210, 1.491842754445841690, 9.504268750180312253 ) ) ;
#339 = DIRECTION ( 'NONE',  ( 0.000000000000000000, 0.000000000000000000, 1.000000000000000000 ) ) ;
#340 = CARTESIAN_POINT ( 'NONE',  ( 19.99999999999999645, -46.17500197033019305, -55.24372537266444283 ) ) ;
#341 = DIRECTION ( 'NONE',  ( -1.000000000000000000, -0.000000000000000000, 0.000000000000000000 ) ) ;
#342 = CARTESIAN_POINT ( 'NONE',  ( 30.00000000000000000, -39.99999999999999289, -52.00000000000000000 ) ) ;
#343 = ORIENTED_EDGE ( 'NONE', *, *, #19126, .T. ) ;
#344 = CARTESIAN_POINT ( 'NONE',  ( 2.870125743571140475, 6.929096493489632635, 4.871512500180315008 ) ) ;
#345 = ORIENTED_EDGE ( 'NONE', *, *, #11654, .T. ) ;
#346 = CARTESIAN_POINT ( 'NONE',  ( 2.163825119083639534E-09, 18.00000000000000000, 19.04770000018031340 ) ) ;
#347 = CARTESIAN_POINT ( 'NONE',  ( 0.000000000000000000, 68.15657073222436679, 23.20952102120305582 ) ) ;
#348 = AXIS2_PLACEMENT_3D ( 'NONE', #20750, #6237, #19174 ) ;
#349 = VERTEX_POINT ( 'NONE', #17246 ) ;
#350 = CARTESIAN_POINT ( 'NONE',  ( 19.99999999999999645, 0.000000000000000000, 0.000000000000000000 ) ) ;
#351 = ORIENTED_EDGE ( 'NONE', *, *, #3136, .F. ) ;
#352 = PRODUCT_DEFINITION_SHAPE ( 'NONE', 'NONE',  #13380 ) ;
#353 = DIRECTION ( 'NONE',  ( 0.000000000000000000, 0.000000000000000000, 1.000000000000000000 ) ) ;
#354 = DIRECTION ( 'NONE',  ( -1.000000000000000000, 0.000000000000000000, 0.000000000000000000 ) ) ;
#355 = EDGE_CURVE ( 'NONE', #16003, #19785, #20624, .T. ) ;
#356 = ORIENTED_EDGE ( 'NONE', *, *, #13998, .F. ) ;
#357 = AXIS2_PLACEMENT_3D ( 'NONE', #9156, #15411, #7774 ) ;
#358 = CARTESIAN_POINT ( 'NONE',  ( 2.870125743571138255, 6.929096493489627306, -10.81838749981969450 ) ) ;
#359 = DIRECTION ( 'NONE',  ( -0.000000000000000000, -1.000000000000000000, -0.000000000000000000 ) ) ;
#360 = VECTOR ( 'NONE', #15398, 1000.000000000000000 ) ;
#361 = CARTESIAN_POINT ( 'NONE',  ( 7.902369978624329327, 7.902369976724401113, 5.889484750647431710 ) ) ;
#362 = ORIENTED_EDGE ( 'NONE', *, *, #16789, .T. ) ;
#363 = DIRECTION ( 'NONE',  ( -1.000000000000000000, 0.000000000000000000, 0.000000000000000000 ) ) ;
#364 = LINE ( 'NONE', #2170, #17294 ) ;
#365 = ORIENTED_EDGE ( 'NONE', *, *, #15296, .T. ) ;
#366 = EDGE_CURVE ( 'NONE', #1598, #19691, #9182, .T. ) ;
#367 = DIRECTION ( 'NONE',  ( -1.000000000000000000, 0.000000000000000000, 0.000000000000000000 ) ) ;
#368 = EDGE_LOOP ( 'NONE', ( #9390, #15256, #3341, #1635, #4917, #19563, #12589, #1221 ) ) ;
#369 = CARTESIAN_POINT ( 'NONE',  ( 18.00000000043041126, 3.580422610670019434, 13.58901875018031369 ) ) ;
#370 = CARTESIAN_POINT ( 'NONE',  ( -9.850000000000006750, 0.000000000000000000, -43.00000000000000000 ) ) ;
#371 = CARTESIAN_POINT ( 'NONE',  ( 2.500000000000000000, 2.629050547790028946E-15, 2.042000000000000259 ) ) ;
#372 = EDGE_LOOP ( 'NONE', ( #18195, #3696, #3655, #20079 ) ) ;
#373 = CYLINDRICAL_SURFACE ( 'NONE', #5994, 27.60000000002760245 ) ;
#374 = CIRCLE ( 'NONE', #15611, 72.00000000007199219 ) ;
#375 = ORIENTED_EDGE ( 'NONE', *, *, #7332, .F. ) ;
#376 = DIRECTION ( 'NONE',  ( 0.000000000000000000, 0.000000000000000000, -1.000000000000000000 ) ) ;
#377 = DIRECTION ( 'NONE',  ( 0.000000000000000000, 0.9422609221188190665, 0.3348796121709901041 ) ) ;
#378 = ORIENTED_EDGE ( 'NONE', *, *, #18023, .T. ) ;
#379 = CARTESIAN_POINT ( 'NONE',  ( 2.000000000000027089, 3.464101615137739731, -5.600000000000000533 ) ) ;
#380 = EDGE_CURVE ( 'NONE', #16309, #18776, #7801, .T. ) ;
#381 = EDGE_CURVE ( 'NONE', #14573, #1539, #14276, .T. ) ;
#382 = CARTESIAN_POINT ( 'NONE',  ( 0.000000000000000000, 0.000000000000000000, 0.000000000000000000 ) ) ;
#383 = APPLICATION_PROTOCOL_DEFINITION ( 'draft international standard', 'automotive_design', 1998, #3554 ) ;
#384 = CARTESIAN_POINT ( 'NONE',  ( 16.62983158437509701, -6.888301784570740161, -23.22738749981969519 ) ) ;
#386 = EDGE_LOOP ( 'NONE', ( #256, #15572, #3501, #7705 ) ) ;
#385 = AXIS2_PLACEMENT_3D ( 'NONE', #5569, #16920, #8861 ) ;
#387 = DIRECTION ( 'NONE',  ( 0.000000000000000000, 0.000000000000000000, -1.000000000000000000 ) ) ;
#388 = EDGE_CURVE ( 'NONE', #1886, #2751, #11934, .T. ) ;
#389 = EDGE_LOOP ( 'NONE', ( #1248, #17136 ) ) ;
#390 = ADVANCED_FACE ( 'NONE', ( #4205 ), #11548, .F. ) ;
#391 = FACE_BOUND ( 'NONE', #20016, .T. ) ;
#392 = CARTESIAN_POINT ( 'NONE',  ( 2.943691928843430450, 14.79893867722910095, -20.21451066848093703 ) ) ;
#393 = DIRECTION ( 'NONE',  ( -0.000000000000000000, -0.000000000000000000, 1.000000000000000000 ) ) ;
#394 = ORIENTED_EDGE ( 'NONE', *, *, #20877, .T. ) ;
#395 = CYLINDRICAL_SURFACE ( 'NONE', #13106, 2.649999999999993694 ) ;
#396 = CARTESIAN_POINT ( 'NONE',  ( 3.599999999999909051, -10.82531754730554496, 169.0000000000000000 ) ) ;
#397 = ORIENTED_EDGE ( 'NONE', *, *, #2654, .T. ) ;
#398 = CIRCLE ( 'NONE', #17331, 10.00000000000000178 ) ;
#399 = EDGE_CURVE ( 'NONE', #15833, #20459, #9087, .T. ) ;
#400 = CARTESIAN_POINT ( 'NONE',  ( 16.55500000000001393, 0.000000000000000000, 0.000000000000000000 ) ) ;
#401 = VECTOR ( 'NONE', #13393, 1000.000000000000000 ) ;
#402 = ORIENTED_EDGE ( 'NONE', *, *, #6479, .T. ) ;
#403 = CARTESIAN_POINT ( 'NONE',  ( 6.250000000000054179, 10.82531754730546147, 40.00000000000000000 ) ) ;
#404 = CARTESIAN_POINT ( 'NONE',  ( 6.888301780572505528, -16.62983158603121581, 4.321137500180309843 ) ) ;
#405 = VERTEX_POINT ( 'NONE', #11404 ) ;
#406 = AXIS2_PLACEMENT_3D ( 'NONE', #17598, #16302, #3065 ) ;
#407 = ORIENTED_EDGE ( 'NONE', *, *, #13428, .F. ) ;
#408 = CARTESIAN_POINT ( 'NONE',  ( 48.80907113954126686, -2.531514235868165041, -83.66807691527674251 ) ) ;
#409 = EDGE_CURVE ( 'NONE', #16888, #19366, #720, .T. ) ;
#410 = EDGE_CURVE ( 'NONE', #20805, #2701, #9805, .T. ) ;
#411 = CARTESIAN_POINT ( 'NONE',  ( -27.96694501150314593, -24.74873734152930993, -120.0000000000000142 ) ) ;
#412 = CARTESIAN_POINT ( 'NONE',  ( 0.000000000000000000, -31.98952867950364265, 56.39803944231574206 ) ) ;
#413 = SURFACE_STYLE_USAGE ( .BOTH. , #8153 ) ;
#414 = B_SPLINE_CURVE_WITH_KNOTS ( 'NONE', 3,
 ( #19492, #9752, #16310, #4765, #6760, #9842, #11534, #9653 ),
 .UNSPECIFIED., .F., .F.,
 ( 4, 2, 2, 4 ),
 ( 0.000000000000000000, 0.005433550342329228865, 0.008150325513493860211, 0.01086710068465849069 ),
 .UNSPECIFIED. ) ;
#415 = CARTESIAN_POINT ( 'NONE',  ( -3.580422614997675890, -17.99999999956958519, 16.53433125018031191 ) ) ;
#417 = ADVANCED_FACE ( 'NONE', ( #11194 ), #8420, .T. ) ;
#416 = PRESENTATION_STYLE_ASSIGNMENT (( #4000 ) ) ;
#418 = CARTESIAN_POINT ( 'NONE',  ( -7.500000000000007994, 9.015942588607339023E-10, 11.35120000018031661 ) ) ;
#419 = AXIS2_PLACEMENT_3D ( 'NONE', #4743, #6227, #16194 ) ;
#420 = AXIS2_PLACEMENT_3D ( 'NONE', #16229, #16325, #1815 ) ;
#421 = CARTESIAN_POINT ( 'NONE',  ( -4.276731815070945686, -10.32494394706615637, 2.890202749713199459 ) ) ;
#422 = AXIS2_PLACEMENT_3D ( 'NONE', #16823, #3876, #10248 ) ;
#423 = CIRCLE ( 'NONE', #18039, 2.500000000000000444 ) ;
#424 = CARTESIAN_POINT ( 'NONE',  ( 19.99999999999999645, 0.000000000000000000, 0.000000000000000000 ) ) ;
#425 = CARTESIAN_POINT ( 'NONE',  ( 5.200000000000002842, 0.000000000000000000, 0.000000000000000000 ) ) ;
#426 = EDGE_LOOP ( 'NONE', ( #46, #12533, #18701, #17009 ) ) ;
#427 = DIRECTION ( 'NONE',  ( -0.000000000000000000, -0.000000000000000000, 1.000000000000000000 ) ) ;
#428 = CARTESIAN_POINT ( 'NONE',  ( 3.580422610670020322, -18.00000000043041126, 15.94526875018031298 ) ) ;
#429 = PLANE ( 'NONE',  #8031 ) ;
#430 = AXIS2_PLACEMENT_3D ( 'NONE', #20619, #19149, #20718 ) ;
#431 = ADVANCED_FACE ( 'NONE', ( #19348 ), #12806, .T. ) ;
#432 = ORIENTED_EDGE ( 'NONE', *, *, #14930, .F. ) ;
#433 = EDGE_CURVE ( 'NONE', #17850, #17173, #15609, .T. ) ;
#434 = CARTESIAN_POINT ( 'NONE',  ( 0.000000000000000000, -51.43306257653170377, 40.15061736769546741 ) ) ;
#435 = ORIENTED_EDGE ( 'NONE', *, *, #9307, .T. ) ;
#436 = ADVANCED_FACE ( 'NONE', ( #3137 ), #6413, .T. ) ;
#437 = CARTESIAN_POINT ( 'NONE',  ( 0.000000000000000000, -23.08379033237309841, -61.02926039941459635 ) ) ;
#438 = CARTESIAN_POINT ( 'NONE',  ( 33.67895669406915715, -28.64151946020273343, 73.35365590739139918 ) ) ;
#439 = EDGE_LOOP ( 'NONE', ( #20238, #7654, #8119, #10471 ) ) ;
#440 = VERTEX_POINT ( 'NONE', #3545 ) ;
#441 = CARTESIAN_POINT ( 'NONE',  ( 19.99999999999999645, -14.55863677812166124, 63.60407295269099137 ) ) ;
#442 = CIRCLE ( 'NONE', #19390, 2.099999999999997868 ) ;
#443 = CIRCLE ( 'NONE', #7543, 27.60000000002760245 ) ;
#444 = AXIS2_PLACEMENT_3D ( 'NONE', #3077, #18985, #4249 ) ;
#445 = ADVANCED_FACE ( 'NONE', ( #16181 ), #20833, .T. ) ;
#446 = AXIS2_PLACEMENT_3D ( 'NONE', #8844, #4070, #16804 ) ;
#447 = PRESENTATION_STYLE_ASSIGNMENT (( #16544 ) ) ;
#448 = DIRECTION ( 'NONE',  ( 0.000000000000000000, -0.4999999999999993894, 0.8660254037844389297 ) ) ;
#449 = DIRECTION ( 'NONE',  ( 0.000000000000000000, 0.000000000000000000, -1.000000000000000000 ) ) ;
#450 = CIRCLE ( 'NONE', #13996, 27.60000000002760245 ) ;
#451 = CARTESIAN_POINT ( 'NONE',  ( 4.248408730893245888, 6.358192987158590270, 17.75114375018031510 ) ) ;
#452 = DIRECTION ( 'NONE',  ( 1.000000000000000000, 0.000000000000000000, 0.000000000000000000 ) ) ;
#453 = CYLINDRICAL_SURFACE ( 'NONE', #5418, 27.60000000002759890 ) ;
#454 = AXIS2_PLACEMENT_3D ( 'NONE', #4721, #15855, #10975 ) ;
#455 = DIRECTION ( 'NONE',  ( 1.000000000000000000, 0.000000000000000000, 0.000000000000000000 ) ) ;
#456 = DIRECTION ( 'NONE',  ( -0.000000000000000000, -0.000000000000000000, 1.000000000000000000 ) ) ;
#457 = AXIS2_PLACEMENT_3D ( 'NONE', #13399, #8610, #18470 ) ;
#458 = ORIENTED_EDGE ( 'NONE', *, *, #13711, .F. ) ;
#459 = DIRECTION ( 'NONE',  ( 1.000000000000000000, 0.000000000000000000, 0.000000000000000000 ) ) ;
#460 = ORIENTED_EDGE ( 'NONE', *, *, #8185, .F. ) ;
#461 = DIRECTION ( 'NONE',  ( -1.836909530733573776E-16, 1.000000000000000000, 0.000000000000000000 ) ) ;
#462 = DIRECTION ( 'NONE',  ( 0.000000000000000000, -0.1361666490962330500, -0.9906859460363326431 ) ) ;
#463 = ORIENTED_EDGE ( 'NONE', *, *, #15828, .T. ) ;
#464 = CARTESIAN_POINT ( 'NONE',  ( 2.500000000000000000, 1.178949249685212974, -2.042000000000001148 ) ) ;
#465 = ORIENTED_EDGE ( 'NONE', *, *, #10809, .T. ) ;
#466 = CARTESIAN_POINT ( 'NONE',  ( 6.250000000000054179, 10.82531754730546147, 126.0000000000000000 ) ) ;
#467 = DIRECTION ( 'NONE',  ( -1.000000000000000000, -0.000000000000000000, -0.000000000000000000 ) ) ;
#468 = AXIS2_PLACEMENT_3D ( 'NONE', #13809, #3821, #7105 ) ;
#469 = ORIENTED_EDGE ( 'NONE', *, *, #6864, .F. ) ;
#470 = AXIS2_PLACEMENT_3D ( 'NONE', #11831, #16705, #14913 ) ;
#471 = CIRCLE ( 'NONE', #1159, 27.60000000002759535 ) ;
#472 = DIRECTION ( 'NONE',  ( -1.000000000000000000, 0.000000000000000000, 0.000000000000000000 ) ) ;
#473 = CARTESIAN_POINT ( 'NONE',  ( -10.19618095047497874, 15.25966317163202746, -10.11089374981968980 ) ) ;
#474 = AXIS2_PLACEMENT_3D ( 'NONE', #7316, #10187, #8701 ) ;
#475 = FACE_OUTER_BOUND ( 'NONE', #5629, .T. ) ;
#476 = AXIS2_PLACEMENT_3D ( 'NONE', #11866, #6887, #5498 ) ;
#477 = DIRECTION ( 'NONE',  ( -1.000000000000000000, -0.000000000000000000, -0.000000000000000000 ) ) ;
#478 =( REPRESENTATION_RELATIONSHIP ('NONE','NONE', #13739, #12383 ) REPRESENTATION_RELATIONSHIP_WITH_TRANSFORMATION ( #7901 )SHAPE_REPRESENTATION_RELATIONSHIP( ) );
#479 = CARTESIAN_POINT ( 'NONE',  ( -9.474249098604513364, -6.330490856366295382, 10.89651600064742887 ) ) ;
#480 = ORIENTED_EDGE ( 'NONE', *, *, #6619, .T. ) ;
#481 = CARTESIAN_POINT ( 'NONE',  ( -3.673643420401911275, -2.497823135841290565, -5.351519936624989704 ) ) ;
#482 = EDGE_CURVE ( 'NONE', #14903, #18469, #1761, .T. ) ;
#483 = CARTESIAN_POINT ( 'NONE',  ( 3.678949249685231848, 0.000000000000000000, 0.000000000000000000 ) ) ;
#484 = ORIENTED_EDGE ( 'NONE', *, *, #9111, .T. ) ;
#485 = CIRCLE ( 'NONE', #12331, 27.60000000002759535 ) ;
#486 = FACE_OUTER_BOUND ( 'NONE', #14457, .T. ) ;
#487 = ORIENTED_EDGE ( 'NONE', *, *, #16093, .F. ) ;
#488 = CARTESIAN_POINT ( 'NONE',  ( 15.25966317163202746, 10.19618095047498407, 12.99995625018031475 ) ) ;
#489 = CARTESIAN_POINT ( 'NONE',  ( -31.75000000000000000, 11.49999999999999467, 0.000000000000000000 ) ) ;
#490 = PLANE ( 'NONE',  #10357 ) ;
#491 = ORIENTED_EDGE ( 'NONE', *, *, #7031, .F. ) ;
#492 = AXIS2_PLACEMENT_3D ( 'NONE', #3114, #20504, #7782 ) ;
#493 = CARTESIAN_POINT ( 'NONE',  ( 19.99999999999999645, 58.44960523466241398, 28.06621538408611016 ) ) ;
#494 = ORIENTED_EDGE ( 'NONE', *, *, #12195, .F. ) ;
#495 = CARTESIAN_POINT ( 'NONE',  ( 50.00000000000000000, 36.35083268962915781, -50.00000000000000000 ) ) ;
#496 = CIRCLE ( 'NONE', #12347, 72.00000000007199219 ) ;
#497 = ORIENTED_EDGE ( 'NONE', *, *, #16576, .F. ) ;
#498 = CARTESIAN_POINT ( 'NONE',  ( 7.500000000000000000, 9.184850993605147944E-16, 40.00000000000000000 ) ) ;
#499 = FACE_OUTER_BOUND ( 'NONE', #3244, .T. ) ;
#500 = PRODUCT_CONTEXT ( 'NONE', #4657, 'mechanical' ) ;
#501 = CARTESIAN_POINT ( 'NONE',  ( 10.46442989454075700, 10.46442989202484419, 23.98716691884155239 ) ) ;
#502 = ORIENTED_EDGE ( 'NONE', *, *, #2819, .T. ) ;
#503 = CIRCLE ( 'NONE', #7250, 27.60000000002759890 ) ;
#504 = EDGE_CURVE ( 'NONE', #197, #10395, #14123, .T. ) ;
#505 = CARTESIAN_POINT ( 'NONE',  ( 6.249999999999902300, -10.82531754730554496, 126.0000000000000000 ) ) ;
#506 =( NAMED_UNIT ( * ) PLANE_ANGLE_UNIT ( ) SI_UNIT ( $, .RADIAN. ) );
#507 = CARTESIAN_POINT ( 'NONE',  ( 18.00000000043040771, 3.580422610670018546, 21.10941875018031055 ) ) ;
#508 = DIRECTION ( 'NONE',  ( 0.000000000000000000, 0.000000000000000000, -1.000000000000000000 ) ) ;
#509 = ADVANCED_FACE ( 'NONE', ( #15936 ), #19629, .T. ) ;
#510 = VERTEX_POINT ( 'NONE', #11579 ) ;
#511 = LINE ( 'NONE', #16826, #13773 ) ;
#512 = DIRECTION ( 'NONE',  ( -0.000000000000000000, 0.000000000000000000, 1.000000000000000000 ) ) ;
#513 = EDGE_LOOP ( 'NONE', ( #7968, #13758, #16479, #7513 ) ) ;
#514 = CARTESIAN_POINT ( 'NONE',  ( 5.200000000000002842, 0.000000000000000000, 0.000000000000000000 ) ) ;
#515 = ORIENTED_EDGE ( 'NONE', *, *, #13376, .F. ) ;
#516 = CIRCLE ( 'NONE', #19452, 27.60000000002760245 ) ;
#517 = DIRECTION ( 'NONE',  ( -1.000000000000000000, -0.000000000000000000, 0.000000000000000000 ) ) ;
#518 = CARTESIAN_POINT ( 'NONE',  ( 17.99999999999999645, -2.163824016901520184E-09, 2.553950000180309932 ) ) ;
#519 = ORIENTED_EDGE ( 'NONE', *, *, #3660, .T. ) ;
#520 = VERTEX_POINT ( 'NONE', #20918 ) ;
#521 = DIRECTION ( 'NONE',  ( -0.000000000000000000, -0.000000000000000000, 1.000000000000000000 ) ) ;
#522 = EDGE_CURVE ( 'NONE', #9436, #1433, #1651, .T. ) ;
#523 = LINE ( 'NONE', #11956, #5988 ) ;
#524 = CYLINDRICAL_SURFACE ( 'NONE', #10905, 80.00000000000000000 ) ;
#525 = CARTESIAN_POINT ( 'NONE',  ( 10.19618095047498052, -15.25966317163203456, 15.35620625018031049 ) ) ;
#526 = UNCERTAINTY_MEASURE_WITH_UNIT (LENGTH_MEASURE( 1.000000000000000082E-05 ), #19696, 'distance_accuracy_value', 'NONE');
#527 = DIRECTION ( 'NONE',  ( -1.000000000000000000, 0.000000000000000000, 0.000000000000000000 ) ) ;
#528 = CARTESIAN_POINT ( 'NONE',  ( 4.248408730893249441, 6.358192987158595599, 5.166043750180316252 ) ) ;
#529 = VECTOR ( 'NONE', #18916, 1000.000000000000000 ) ;
#530 = CARTESIAN_POINT ( 'NONE',  ( -4.276731812588563386, 10.32494394809438987, -12.42542225028680214 ) ) ;
#531 = PRODUCT_DEFINITION_SHAPE ( 'NONE', 'NONE',  #10520 ) ;
#532 = CARTESIAN_POINT ( 'NONE',  ( -31.75000000000000000, 0.000000000000000000, 0.000000000000000000 ) ) ;
#533 = DIRECTION ( 'NONE',  ( 1.000000000000000000, 0.000000000000000000, -0.000000000000000000 ) ) ;
#534 = ADVANCED_FACE ( 'NONE', ( #19430 ), #11383, .F. ) ;
#535 = ORIENTED_EDGE ( 'NONE', *, *, #11183, .F. ) ;
#536 = CARTESIAN_POINT ( 'NONE',  ( 0.000000000000000000, 0.000000000000000000, 126.0000000000000000 ) ) ;
#537 = EDGE_CURVE ( 'NONE', #13895, #14604, #14603, .T. ) ;
#538 = CARTESIAN_POINT ( 'NONE',  ( 10.19618095414378800, 15.25966316918061416, 2.985893750180313333 ) ) ;
#539 = CARTESIAN_POINT ( 'NONE',  ( 0.000000000000000000, 0.000000000000000000, -120.0000000000000142 ) ) ;
#540 = VERTEX_POINT ( 'NONE', #14767 ) ;
#541 = DIRECTION ( 'NONE',  ( 1.000000000000000000, 0.000000000000000000, -0.000000000000000000 ) ) ;
#542 = ORIENTED_EDGE ( 'NONE', *, *, #11407, .F. ) ;
#543 = CARTESIAN_POINT ( 'NONE',  ( -15.15000000000000036, 0.000000000000000000, 166.0000000000000000 ) ) ;
#544 = DIRECTION ( 'NONE',  ( 0.000000000000000000, 0.000000000000000000, -1.000000000000000000 ) ) ;
#545 = CIRCLE ( 'NONE', #6954, 27.60000000002759890 ) ;
#546 = ADVANCED_FACE ( 'NONE', ( #140 ), #19233, .F. ) ;
#547 = ORIENTED_EDGE ( 'NONE', *, *, #16992, .T. ) ;
#548 = EDGE_CURVE ( 'NONE', #12159, #1568, #1422, .T. ) ;
#549 = ORIENTED_EDGE ( 'NONE', *, *, #7060, .T. ) ;
#550 = DIRECTION ( 'NONE',  ( -1.000000000000000000, -0.000000000000000000, -0.000000000000000000 ) ) ;
#551 = VECTOR ( 'NONE', #6875, 1000.000000000000000 ) ;
#552 = DIRECTION ( 'NONE',  ( 0.000000000000000000, -0.000000000000000000, 1.000000000000000000 ) ) ;
#553 = DIRECTION ( 'NONE',  ( 0.000000000000000000, 0.000000000000000000, -1.000000000000000000 ) ) ;
#554 = EDGE_CURVE ( 'NONE', #1571, #4727, #3426, .T. ) ;
#555 = CARTESIAN_POINT ( 'NONE',  ( -9.015947181032828388E-10, -7.500000000000000888, -6.694949999819691300 ) ) ;
#556 = AXIS2_PLACEMENT_3D ( 'NONE', #16543, #2028, #19617 ) ;
#557 = LINE ( 'NONE', #11880, #11849 ) ;
#558 = LINE ( 'NONE', #11785, #13211 ) ;
#559 = CARTESIAN_POINT ( 'NONE',  ( 7.500000000000000000, 9.184850993605147944E-16, 166.0000000000000000 ) ) ;
#560 = CARTESIAN_POINT ( 'NONE',  ( -44.00000000000000000, -85.00000000000000000, -14.50000000000000533 ) ) ;
#561 = CIRCLE ( 'NONE', #8670, 72.00000000007199219 ) ;
#562 = CIRCLE ( 'NONE', #15113, 72.00000000007199219 ) ;
#563 = ORIENTED_EDGE ( 'NONE', *, *, #3533, .T. ) ;
#564 = FACE_OUTER_BOUND ( 'NONE', #13636, .T. ) ;
#565 = EDGE_CURVE ( 'NONE', #16083, #12428, #19535, .T. ) ;
#566 = ORIENTED_EDGE ( 'NONE', *, *, #15947, .T. ) ;
#567 = CARTESIAN_POINT ( 'NONE',  ( -3.580422610670018546, 18.00000000043041126, 9.328168750180314106 ) ) ;
#568 = CARTESIAN_POINT ( 'NONE',  ( 19.99999999999999645, 64.80702306891095077, 7.581672767546655756 ) ) ;
#569 = ORIENTED_EDGE ( 'NONE', *, *, #18170, .F. ) ;
#570 = CARTESIAN_POINT ( 'NONE',  ( 0.000000000000000000, 0.000000000000000000, -40.00000000000000000 ) ) ;
#571 = ORIENTED_EDGE ( 'NONE', *, *, #18719, .T. ) ;
#572 = EDGE_CURVE ( 'NONE', #17279, #5928, #1748, .T. ) ;
#573 = CARTESIAN_POINT ( 'NONE',  ( 44.19470160754491417, -125.5384278435233085, 83.11447728151287606 ) ) ;
#574 = CARTESIAN_POINT ( 'NONE',  ( 30.00000000000000000, 4.299168419249259188, -90.00000000000001421 ) ) ;
#575 = AXIS2_PLACEMENT_3D ( 'NONE', #4476, #9146, #4374 ) ;
#576 = ORIENTED_EDGE ( 'NONE', *, *, #8396, .F. ) ;
#577 = VECTOR ( 'NONE', #11848, 1000.000000000000000 ) ;
#578 = CARTESIAN_POINT ( 'NONE',  ( 50.00000000000000000, -30.00000000000000711, 44.99999999999998579 ) ) ;
#579 = CARTESIAN_POINT ( 'NONE',  ( -12.72792205982779556, 12.72792206288790773, -0.9804249998196894467 ) ) ;
#580 = CARTESIAN_POINT ( 'NONE',  ( 19.99999999999999645, 0.000000000000000000, 0.000000000000000000 ) ) ;
#581 = AXIS2_PLACEMENT_3D ( 'NONE', #14078, #19049, #12260 ) ;
#582 = CARTESIAN_POINT ( 'NONE',  ( 0.000000000000000000, 0.000000000000000000, -81.99999999999998579 ) ) ;
#583 = CARTESIAN_POINT ( 'NONE',  ( -11.17563879731705789, 1.343452237168309506E-09, 2.355109750647427891 ) ) ;
#584 = ORIENTED_EDGE ( 'NONE', *, *, #5461, .T. ) ;
#585 = EDGE_CURVE ( 'NONE', #14577, #18338, #19669, .T. ) ;
#586 = CARTESIAN_POINT ( 'NONE',  ( 30.00000000000000000, -85.00000000000000000, 79.99999999999998579 ) ) ;
#587 = LINE ( 'NONE', #20169, #6447 ) ;
#588 = VERTEX_POINT ( 'NONE', #20812 ) ;
#589 = CARTESIAN_POINT ( 'NONE',  ( -10.25561400234657583, -18.90011081285701877, -71.73813932909898483 ) ) ;
#590 = ORIENTED_EDGE ( 'NONE', *, *, #11130, .F. ) ;
#591 = AXIS2_PLACEMENT_3D ( 'NONE', #11419, #8126, #19460 ) ;
#592 = CARTESIAN_POINT ( 'NONE',  ( -6.888301784570738384, -16.62983158437509346, -2.021137499819688266 ) ) ;
#593 = CARTESIAN_POINT ( 'NONE',  ( 19.99999999999999645, 0.000000000000000000, 0.000000000000000000 ) ) ;
#594 = CARTESIAN_POINT ( 'NONE',  ( 0.000000000000000000, 0.000000000000000000, 81.99999999999998579 ) ) ;
#595 = CIRCLE ( 'NONE', #8055, 14.49999999999999822 ) ;
#596 = ORIENTED_EDGE ( 'NONE', *, *, #15835, .F. ) ;
#597 = CARTESIAN_POINT ( 'NONE',  ( -6.929096493489632635, 2.870125743571140919, 11.94026250018031554 ) ) ;
#598 = AXIS2_PLACEMENT_3D ( 'NONE', #6935, #14894, #11405 ) ;
#599 = ORIENTED_EDGE ( 'NONE', *, *, #3122, .F. ) ;
#600 = DIRECTION ( 'NONE',  ( 1.000000000000000000, 0.000000000000000000, 0.000000000000000000 ) ) ;
#601 = EDGE_CURVE ( 'NONE', #3647, #5060, #13252, .T. ) ;
#602 = VECTOR ( 'NONE', #1570, 1000.000000000000000 ) ;
#603 = ORIENTED_EDGE ( 'NONE', *, *, #9501, .T. ) ;
#604 = DIRECTION ( 'NONE',  ( 0.000000000000000000, 1.059758341687649568E-14, -1.000000000000000000 ) ) ;
#605 = VECTOR ( 'NONE', #19751, 1000.000000000000000 ) ;
#606 = CARTESIAN_POINT ( 'NONE',  ( 2.500000000000000000, 0.000000000000000000, 0.000000000000000000 ) ) ;
#607 = CONTEXT_DEPENDENT_SHAPE_REPRESENTATION ( #877, #8641 ) ;
#608 = CARTESIAN_POINT ( 'NONE',  ( 17.99999999956958519, -3.580422614997676778, -23.52191874981969733 ) ) ;
#610 = EDGE_LOOP ( 'NONE', ( #11932, #18314, #16602, #14575, #289 ) ) ;
#609 = AXIS2_PLACEMENT_3D ( 'NONE', #16709, #9927, #8437 ) ;
#611 = DIRECTION ( 'NONE',  ( -1.000000000000000000, 0.000000000000000000, -0.000000000000000000 ) ) ;
#612 = ORIENTED_EDGE ( 'NONE', *, *, #3873, .T. ) ;
#613 = CARTESIAN_POINT ( 'NONE',  ( -54.64999999999999858, -39.99999999999999289, 5.000000000000000000 ) ) ;
#614 = CARTESIAN_POINT ( 'NONE',  ( 8.382925371439627682, 12.54593441562639988, -19.62544816848093276 ) ) ;
#615 = DIRECTION ( 'NONE',  ( 0.000000000000000000, 0.000000000000000000, -1.000000000000000000 ) ) ;
#616 = ORIENTED_EDGE ( 'NONE', *, *, #20084, .T. ) ;
#617 = LINE ( 'NONE', #825, #17851 ) ;
#618 = DIRECTION ( 'NONE',  ( 0.000000000000000000, 0.000000000000000000, 1.000000000000000000 ) ) ;
#619 = ORIENTED_EDGE ( 'NONE', *, *, #11741, .F. ) ;
#620 = LINE ( 'NONE', #13141, #16338 ) ;
#621 = ORIENTED_EDGE ( 'NONE', *, *, #10925, .T. ) ;
#622 = DIRECTION ( 'NONE',  ( 1.000000000000000000, 0.000000000000000000, 0.000000000000000000 ) ) ;
#623 = CARTESIAN_POINT ( 'NONE',  ( 12.72792205982779379, -12.72792206288790950, 3.732075000180308688 ) ) ;
#624 = EDGE_CURVE ( 'NONE', #15909, #5939, #1544, .T. ) ;
#625 = ORIENTED_EDGE ( 'NONE', *, *, #13485, .F. ) ;
#626 = ORIENTED_EDGE ( 'NONE', *, *, #13110, .T. ) ;
#627 = DIRECTION ( 'NONE',  ( -0.000000000000000000, -0.000000000000000000, -1.000000000000000000 ) ) ;
#628 = DIRECTION ( 'NONE',  ( -0.000000000000000000, -0.000000000000000000, 1.000000000000000000 ) ) ;
#629 = CARTESIAN_POINT ( 'NONE',  ( -7.000000000000000888, 10.52400000000000091, 0.000000000000000000 ) ) ;
#630 = FILL_AREA_STYLE_COLOUR ( '', #18791 ) ;
#631 = EDGE_CURVE ( 'NONE', #10778, #3180, #16303, .T. ) ;
#632 = CARTESIAN_POINT ( 'NONE',  ( 4.248408729364579806, -6.358192988180021210, -1.313643749819685347 ) ) ;
#633 = CARTESIAN_POINT ( 'NONE',  ( 2.222972768810837163, -11.17563879758427525, -7.418391000286802317 ) ) ;
#634 = CYLINDRICAL_SURFACE ( 'NONE', #10755, 65.24900000006525147 ) ;
#635 = ORIENTED_EDGE ( 'NONE', *, *, #20904, .T. ) ;
#636 = DIRECTION ( 'NONE',  ( -1.000000000000000000, 0.000000000000000000, 0.000000000000000000 ) ) ;
#637 = CARTESIAN_POINT ( 'NONE',  ( -12.72792206288791128, -12.72792205982779912, -1.432074999819687333 ) ) ;
#638 = FACE_OUTER_BOUND ( 'NONE', #14639, .T. ) ;
#639 = ORIENTED_EDGE ( 'NONE', *, *, #9100, .F. ) ;
#640 = CYLINDRICAL_SURFACE ( 'NONE', #9217, 27.60000000002759890 ) ;
#641 = ORIENTED_EDGE ( 'NONE', *, *, #12600, .T. ) ;
#642 = PLANE ( 'NONE',  #16291 ) ;
#643 = DIRECTION ( 'NONE',  ( 0.000000000000000000, 0.000000000000000000, 1.000000000000000000 ) ) ;
#644 = ORIENTED_EDGE ( 'NONE', *, *, #7272, .T. ) ;
#645 = VERTEX_POINT ( 'NONE', #3417 ) ;
#646 = DIRECTION ( 'NONE',  ( -1.000000000000000000, 0.000000000000000000, 0.000000000000000000 ) ) ;
#647 = CYLINDRICAL_SURFACE ( 'NONE', #5864, 27.60000000002759890 ) ;
#648 = EDGE_CURVE ( 'NONE', #19326, #1518, #3112, .T. ) ;
#649 = EDGE_CURVE ( 'NONE', #14031, #7362, #7493, .T. ) ;
#650 = DIRECTION ( 'NONE',  ( -1.000000000000000000, 0.000000000000000000, 0.000000000000000000 ) ) ;
#651 = CARTESIAN_POINT ( 'NONE',  ( -6.929096494179677101, -2.870125741905209527, -4.927762499819687392 ) ) ;
#652 = DIRECTION ( 'NONE',  ( -1.000000000000000000, 0.000000000000000000, 0.000000000000000000 ) ) ;
#653 = EDGE_CURVE ( 'NONE', #2314, #5904, #10208, .T. ) ;
#654 = DIRECTION ( 'NONE',  ( -1.000000000000000000, -0.000000000000000000, 0.000000000000000000 ) ) ;
#655 = CARTESIAN_POINT ( 'NONE',  ( 150.0000507999999968, 3.872983346207417021, 1.000000000000000000 ) ) ;
#656 = DIRECTION ( 'NONE',  ( 0.000000000000000000, 0.000000000000000000, -1.000000000000000000 ) ) ;
#657 = ORIENTED_EDGE ( 'NONE', *, *, #4143, .T. ) ;
#658 = LINE ( 'NONE', #7216, #18688 ) ;
#659 = VERTEX_POINT ( 'NONE', #6491 ) ;
#660 = CARTESIAN_POINT ( 'NONE',  ( -16.62983158437510056, 6.888301784570729502, -1.569487499819687049 ) ) ;
#661 = CARTESIAN_POINT ( 'NONE',  ( 10.15192380093072089, -18.95599582743659539, 71.71153801002559192 ) ) ;
#662 = ORIENTED_EDGE ( 'NONE', *, *, #17967, .F. ) ;
#663 = CARTESIAN_POINT ( 'NONE',  ( 1.155036213957052500E-14, 4.618802153517020059, -5.599999999999999645 ) ) ;
#664 = ORIENTED_EDGE ( 'NONE', *, *, #16789, .F. ) ;
#665 = DIRECTION ( 'NONE',  ( 1.000000000000000000, 1.836909530733573776E-16, 0.000000000000000000 ) ) ;
#666 = CARTESIAN_POINT ( 'NONE',  ( 0.000000000000000000, -10.77748419466653651, -63.93680186330482940 ) ) ;
#667 = ORIENTED_EDGE ( 'NONE', *, *, #13110, .F. ) ;
#668 = EDGE_CURVE ( 'NONE', #4597, #15761, #8490, .T. ) ;
#669 = FACE_OUTER_BOUND ( 'NONE', #3773, .T. ) ;
#670 = CARTESIAN_POINT ( 'NONE',  ( 10.19618095047497697, -15.25966317163202923, -14.82339374981968838 ) ) ;
#671 = CARTESIAN_POINT ( 'NONE',  ( 9.999999999999998224, 8.857208570069802889, 71.45313048675089362 ) ) ;
#672 = EDGE_CURVE ( 'NONE', #12901, #12906, #658, .T. ) ;
#673 = EDGE_CURVE ( 'NONE', #7171, #9017, #7154, .T. ) ;
#674 = CARTESIAN_POINT ( 'NONE',  ( -15.14999999999999325, 0.000000000000000000, 126.0000000000000000 ) ) ;
#675 = CARTESIAN_POINT ( 'NONE',  ( -10.32494394809439875, -4.276731812588566051, 1.766047250647429845 ) ) ;
#676 = EDGE_LOOP ( 'NONE', ( #14258, #7952, #17095, #1754 ) ) ;
#677 = FACE_OUTER_BOUND ( 'NONE', #6851, .T. ) ;
#678 = EDGE_CURVE ( 'NONE', #18976, #13722, #3439, .T. ) ;
#679 = CARTESIAN_POINT ( 'NONE',  ( 0.000000000000000000, 0.000000000000000000, 0.000000000000000000 ) ) ;
#680 = AXIS2_PLACEMENT_3D ( 'NONE', #4749, #2450, #15271 ) ;
#681 = ORIENTED_EDGE ( 'NONE', *, *, #8710, .T. ) ;
#682 = CARTESIAN_POINT ( 'NONE',  ( 20.42938063014383943, -6.725612673823790466, -79.66382435179507127 ) ) ;
#683 = ORIENTED_EDGE ( 'NONE', *, *, #6446, .T. ) ;
#684 = CARTESIAN_POINT ( 'NONE',  ( 16.62983158437509346, -6.888301784570739272, 14.47261250018031298 ) ) ;
#685 = DIRECTION ( 'NONE',  ( 0.000000000000000000, 0.000000000000000000, 1.000000000000000000 ) ) ;
#686 = DIRECTION ( 'NONE',  ( -1.000000000000000000, 0.000000000000000000, 0.000000000000000000 ) ) ;
#687 = ORIENTED_EDGE ( 'NONE', *, *, #3710, .F. ) ;
#688 = DIRECTION ( 'NONE',  ( 1.000000000000000000, 0.000000000000000000, 0.000000000000000000 ) ) ;
#689 = EDGE_LOOP ( 'NONE', ( #19136, #7856, #17886, #8453 ) ) ;
#690 = LINE ( 'NONE', #15423, #17999 ) ;
#691 = ORIENTED_EDGE ( 'NONE', *, *, #14028, .T. ) ;
#692 = DIRECTION ( 'NONE',  ( -1.000000000000000000, 0.000000000000000000, 0.000000000000000000 ) ) ;
#693 = EDGE_CURVE ( 'NONE', #6207, #18276, #2473, .T. ) ;
#694 = VECTOR ( 'NONE', #20480, 1000.000000000000000 ) ;
#695 = ORIENTED_EDGE ( 'NONE', *, *, #18063, .F. ) ;
#696 = DIRECTION ( 'NONE',  ( -1.000000000000000000, 0.000000000000000000, 0.000000000000000000 ) ) ;
#697 = PRODUCT_DEFINITION_SHAPE ( 'NONE', 'NONE',  #15563 ) ;
#698 = ADVANCED_FACE ( 'NONE', ( #13281 ), #18053, .T. ) ;
#699 = FACE_OUTER_BOUND ( 'NONE', #426, .T. ) ;
#700 = CARTESIAN_POINT ( 'NONE',  ( -8.382925371439629458, -12.54593441562640876, 9.555135668841547414 ) ) ;
#701 = VERTEX_POINT ( 'NONE', #8605 ) ;
#702 = AXIS2_PLACEMENT_3D ( 'NONE', #6719, #16070, #19647 ) ;
#703 = DIRECTION ( 'NONE',  ( 1.000000000000000000, 0.000000000000000000, 0.000000000000000000 ) ) ;
#704 = DIRECTION ( 'NONE',  ( 0.000000000000000000, 0.000000000000000000, 1.000000000000000000 ) ) ;
#705 = CARTESIAN_POINT ( 'NONE',  ( 13.67243654642774686, -5.663308650141536837, -17.56372941848092850 ) ) ;
#706 = DIRECTION ( 'NONE',  ( -1.000000000000000000, 0.000000000000000000, 0.000000000000000000 ) ) ;
#707 = AXIS2_PLACEMENT_3D ( 'NONE', #18906, #15601, #5958 ) ;
#708 = ORIENTED_EDGE ( 'NONE', *, *, #9616, .T. ) ;
#709 = CARTESIAN_POINT ( 'NONE',  ( 6.249999999999902300, -10.82531754730554496, 166.0000000000000000 ) ) ;
#710 = CARTESIAN_POINT ( 'NONE',  ( 7.500000000000000888, -9.015933403756337545E-10, 19.22380000018031154 ) ) ;
#711 = B_SPLINE_CURVE_WITH_KNOTS ( 'NONE', 3,
 ( #7231, #5536, #12223, #13714, #18693, #3841 ),
 .UNSPECIFIED., .F., .F.,
 ( 4, 2, 4 ),
 ( 0.006456566858647394894, 0.007625406818786665576, 0.008794246778925936259 ),
 .UNSPECIFIED. ) ;
#712 = EDGE_LOOP ( 'NONE', ( #17560, #19304, #1121, #19993 ) ) ;
#713 = CARTESIAN_POINT ( 'NONE',  ( 0.2500000000000002220, 0.000000000000000000, 0.000000000000000000 ) ) ;
#714 = VERTEX_POINT ( 'NONE', #2352 ) ;
#715 = FACE_OUTER_BOUND ( 'NONE', #1941, .T. ) ;
#716 = CARTESIAN_POINT ( 'NONE',  ( -17.99999999956958163, 3.580422614997673669, -1.864018749819690957 ) ) ;
#717 = ORIENTED_EDGE ( 'NONE', *, *, #10249, .T. ) ;
#718 = ORIENTED_EDGE ( 'NONE', *, *, #18889, .F. ) ;
#719 = CARTESIAN_POINT ( 'NONE',  ( 24.74873734152916072, 24.74873734152916072, -120.0000000000000142 ) ) ;
#720 = CIRCLE ( 'NONE', #13579, 65.24900000006525147 ) ;
#721 = CARTESIAN_POINT ( 'NONE',  ( -10.00000000000000000, 0.000000000000000000, 0.000000000000000000 ) ) ;
#722 = LINE ( 'NONE', #17049, #1451 ) ;
#723 = VECTOR ( 'NONE', #7308, 1000.000000000000000 ) ;
#724 = CARTESIAN_POINT ( 'NONE',  ( 3.580422614997669228, 17.99999999956958874, 21.24683125018031049 ) ) ;
#725 = PRODUCT_DEFINITION_CONTEXT ( 'detailed design', #8064, 'design' ) ;
#726 = CARTESIAN_POINT ( 'NONE',  ( 0.000000000000000000, 0.000000000000000000, 40.00000000000000000 ) ) ;
#727 = CARTESIAN_POINT ( 'NONE',  ( 6.358192988180019434, 4.248408729364581582, -3.669893749819685969 ) ) ;
#728 = VECTOR ( 'NONE', #758, 1000.000000000000000 ) ;
#729 = CARTESIAN_POINT ( 'NONE',  ( 85.00002539999999840, 0.000000000000000000, -1.000000000000000000 ) ) ;
#730 = EDGE_CURVE ( 'NONE', #14616, #3271, #16555, .T. ) ;
#731 = CARTESIAN_POINT ( 'NONE',  ( 2.222972768810837163, -11.17563879758427525, -16.84339100028680036 ) ) ;
#732 = ADVANCED_FACE ( 'NONE', ( #564 ), #19740, .T. ) ;
#733 =( BOUNDED_CURVE ( )  B_SPLINE_CURVE ( 2, ( #13842, #9074, #18392, #5667, #18606, #12139, #17233, #13732, #10551, #18502, #2287, #16909, #20182, #8744, #597, #4067, #2499 ),
 .UNSPECIFIED., .F., .T. ) 
 B_SPLINE_CURVE_WITH_KNOTS ( ( 3, 2, 2, 2, 2, 2, 2, 2, 3 ),
 ( 0.2000000000038511805, 0.2125000000038511638, 0.2250000000038511749, 0.2375000000038511860, 0.2500000000038511971, 0.2625000000038512082, 0.2750000000038512193, 0.2875000000038511749, 0.3000000000038511860 ),
 .UNSPECIFIED. ) 
 CURVE ( )  GEOMETRIC_REPRESENTATION_ITEM ( )  RATIONAL_B_SPLINE_CURVE ( ( 0.9999999999940800688, 0.9807852804091503618, 1.000000000000000000, 0.9807852804032304306, 1.000000000000000000, 0.9807852804032304306, 1.000000000000000000, 0.9807852804032304306, 1.000000000000000000, 0.9807852804032304306, 1.000000000000000000, 0.9807852804032304306, 1.000000000000000000, 0.9807852804032304306, 1.000000000000000000, 0.9807852803973104994, 1.000000000005919931 ) ) 
 REPRESENTATION_ITEM ( '' )  );
#734 = CARTESIAN_POINT ( 'NONE',  ( 10.00000000000000178, -160.0000000000000000, 66.80000000000001137 ) ) ;
#735 = CONICAL_SURFACE ( 'NONE', #11896, 4.000000000000000000, 1.047197551196595855 ) ;
#736 = CIRCLE ( 'NONE', #20705, 72.00000000007199219 ) ;
#737 = ORIENTED_EDGE ( 'NONE', *, *, #16854, .F. ) ;
#738 = DIRECTION ( 'NONE',  ( 1.000000000000000000, 0.000000000000000000, 0.000000000000000000 ) ) ;
#739 = CARTESIAN_POINT ( 'NONE',  ( 18.00000000043041126, 3.580422610670019434, -5.260981249819686845 ) ) ;
#740 = LINE ( 'NONE', #16744, #4658 ) ;
#741 = AXIS2_PLACEMENT_3D ( 'NONE', #18003, #20868, #12835 ) ;
#742 = VERTEX_POINT ( 'NONE', #7013 ) ;
#743 = DIRECTION ( 'NONE',  ( 0.000000000000000000, 0.000000000000000000, 1.000000000000000000 ) ) ;
#744 = ORIENTED_EDGE ( 'NONE', *, *, #12088, .F. ) ;
#745 = CARTESIAN_POINT ( 'NONE',  ( 19.99999999999999645, 31.17893654894229982, 57.31758819669181548 ) ) ;
#746 = CARTESIAN_POINT ( 'NONE',  ( 2.500000000000000000, 0.000000000000000000, 0.000000000000000000 ) ) ;
#747 = ORIENTED_EDGE ( 'NONE', *, *, #9656, .T. ) ;
#748 =( GEOMETRIC_REPRESENTATION_CONTEXT ( 3 ) GLOBAL_UNCERTAINTY_ASSIGNED_CONTEXT ( ( #20442 ) ) GLOBAL_UNIT_ASSIGNED_CONTEXT ( ( #18267, #8034, #11319 ) ) REPRESENTATION_CONTEXT ( 'NONE', 'WORKASPACE' ) );
#749 = ORIENTED_EDGE ( 'NONE', *, *, #1732, .F. ) ;
#750 = DIRECTION ( 'NONE',  ( -1.000000000000000000, 0.000000000000000000, 0.000000000000000000 ) ) ;
#751 = CYLINDRICAL_SURFACE ( 'NONE', #17029, 3.199999999999994404 ) ;
#752 = CIRCLE ( 'NONE', #4129, 72.00000000007199219 ) ;
#753 = VECTOR ( 'NONE', #11122, 1000.000000000000000 ) ;
#754 = CIRCLE ( 'NONE', #9564, 27.60000000002760601 ) ;
#755 = DIRECTION ( 'NONE',  ( -1.000000000000000000, -0.000000000000000000, 0.000000000000000000 ) ) ;
#756 = VECTOR ( 'NONE', #17494, 1000.000000000000000 ) ;
#757 = CARTESIAN_POINT ( 'NONE',  ( 6.358192987158590270, -4.248408730893245000, 1.257393750180312741 ) ) ;
#758 = DIRECTION ( 'NONE',  ( 1.000000000000000000, 0.000000000000000000, -0.000000000000000000 ) ) ;
#759 = CARTESIAN_POINT ( 'NONE',  ( 4.999999999999997335, 5.204748896376250699E-16, -4.250000000000000000 ) ) ;
#760 = DIRECTION ( 'NONE',  ( -0.000000000000000000, -0.000000000000000000, 1.000000000000000000 ) ) ;
#761 = LINE ( 'NONE', #10413, #12310 ) ;
#762 = ORIENTED_EDGE ( 'NONE', *, *, #14410, .F. ) ;
#763 = CARTESIAN_POINT ( 'NONE',  ( -5.303300858261589035, 5.303300859536635770, 3.104325000180315541 ) ) ;
#764 = VERTEX_POINT ( 'NONE', #3824 ) ;
#765 = CARTESIAN_POINT ( 'NONE',  ( 15.25966316918061416, -10.19618095414378622, 12.86254375018031304 ) ) ;
#766 = LINE ( 'NONE', #10420, #4559 ) ;
#767 = AXIS2_PLACEMENT_3D ( 'NONE', #7150, #12247, #15530 ) ;
#768 = ORIENTED_EDGE ( 'NONE', *, *, #3979, .F. ) ;
#769 = EDGE_CURVE ( 'NONE', #12727, #12459, #736, .T. ) ;
#770 = CIRCLE ( 'NONE', #17360, 17.00000000000004619 ) ;
#771 = DIRECTION ( 'NONE',  ( 0.000000000000000000, -1.287488025362403787E-15, -1.000000000000000000 ) ) ;
#772 = ORIENTED_EDGE ( 'NONE', *, *, #14173, .F. ) ;
#773 = FACE_OUTER_BOUND ( 'NONE', #9225, .T. ) ;
#774 = CARTESIAN_POINT ( 'NONE',  ( 6.250000000000054179, 10.82531754730546147, 166.0000000000000000 ) ) ;
#775 = AXIS2_PLACEMENT_3D ( 'NONE', #1152, #12379, #14081 ) ;
#776 = ORIENTED_EDGE ( 'NONE', *, *, #3954, .F. ) ;
#777 = CARTESIAN_POINT ( 'NONE',  ( -7.500000000000009770, -1.491842754878800248, -17.21833124991220743 ) ) ;
#778 = EDGE_CURVE ( 'NONE', #4723, #14352, #12593, .T. ) ;
#779 = AXIS2_PLACEMENT_3D ( 'NONE', #17662, #11494, #3132 ) ;
#780 = CYLINDRICAL_SURFACE ( 'NONE', #9366, 27.60000000002759890 ) ;
#781 = CARTESIAN_POINT ( 'NONE',  ( 15.25966316918061239, -10.19618095414378445, -5.987456249819691045 ) ) ;
#782 = DIRECTION ( 'NONE',  ( 0.000000000000000000, 0.000000000000000000, 1.000000000000000000 ) ) ;
#783 = EDGE_CURVE ( 'NONE', #100, #8208, #15180, .T. ) ;
#784 = CARTESIAN_POINT ( 'NONE',  ( 0.000000000000000000, 38.22257254261740655, 61.01667762370151848 ) ) ;
#785 = CARTESIAN_POINT ( 'NONE',  ( -10.32494394809439875, -4.276731812588566051, -7.658952749352573974 ) ) ;
#786 = CIRCLE ( 'NONE', #7897, 0.06721999999999891950 ) ;
#788 = VERTEX_POINT ( 'NONE', #18252 ) ;
#787 = CIRCLE ( 'NONE', #16695, 65.24900000006526568 ) ;
#789 = FILL_AREA_STYLE_COLOUR ( '', #16102 ) ;
#790 = DIRECTION ( 'NONE',  ( -1.000000000000000000, 0.000000000000000000, 0.000000000000000000 ) ) ;
#791 = ORIENTED_EDGE ( 'NONE', *, *, #11962, .T. ) ;
#792 = CARTESIAN_POINT ( 'NONE',  ( -6.110423144575273469, -20.66992657861278460, -70.93137971084412641 ) ) ;
#793 = ORIENTED_EDGE ( 'NONE', *, *, #6745, .F. ) ;
#794 = CARTESIAN_POINT ( 'NONE',  ( -3.580422610670018546, 18.00000000043041126, 11.23276875018031440 ) ) ;
#795 = CARTESIAN_POINT ( 'NONE',  ( 2.500000000000000000, -2.357898499370432610, 3.252606517456513302E-15 ) ) ;
#796 = CARTESIAN_POINT ( 'NONE',  ( 19.99999999999999645, 0.000000000000000000, 0.000000000000000000 ) ) ;
#797 = VECTOR ( 'NONE', #13935, 1000.000000000000000 ) ;
#798 = VERTEX_POINT ( 'NONE', #3718 ) ;
#799 = EDGE_CURVE ( 'NONE', #18653, #12132, #3118, .T. ) ;
#800 = CARTESIAN_POINT ( 'NONE',  ( 2.500000000000000000, -2.357898499370432610, 3.252606517456513302E-15 ) ) ;
#801 = ORIENTED_EDGE ( 'NONE', *, *, #7784, .T. ) ;
#802 = DIRECTION ( 'NONE',  ( 0.000000000000000000, -0.7308359642781301346, 0.6825531432186475733 ) ) ;
#803 = EDGE_CURVE ( 'NONE', #3394, #12901, #13494, .T. ) ;
#804 = ORIENTED_EDGE ( 'NONE', *, *, #7119, .F. ) ;
#805 = AXIS2_PLACEMENT_3D ( 'NONE', #12015, #3844, #1003 ) ;
#806 = CYLINDRICAL_SURFACE ( 'NONE', #17716, 72.00000000007199219 ) ;
#807 = AXIS2_PLACEMENT_3D ( 'NONE', #10287, #13262, #8585 ) ;
#808 = EDGE_CURVE ( 'NONE', #12190, #3649, #18001, .T. ) ;
#809 = CARTESIAN_POINT ( 'NONE',  ( -30.00000000000000000, -97.49621075554985339, 111.6458212409894486 ) ) ;
#810 = CARTESIAN_POINT ( 'NONE',  ( -30.00000000000000000, -85.00000000000000000, -1.040949779275250179E-14 ) ) ;
#811 = CONTEXT_DEPENDENT_SHAPE_REPRESENTATION ( #20771, #18291 ) ;
#812 = CIRCLE ( 'NONE', #14370, 72.00000000007199219 ) ;
#813 = CARTESIAN_POINT ( 'NONE',  ( 14.79893867758297610, -1.779016607511492805E-09, 25.16529191884155026 ) ) ;
#814 = AXIS2_PLACEMENT_3D ( 'NONE', #311, #5176, #18637 ) ;
#815 = ORIENTED_EDGE ( 'NONE', *, *, #9394, .T. ) ;
#816 = LINE ( 'NONE', #10243, #8539 ) ;
#817 = ORIENTED_EDGE ( 'NONE', *, *, #10804, .T. ) ;
#818 = ADVANCED_FACE ( 'NONE', ( #18673 ), #15389, .F. ) ;
#819 = DIRECTION ( 'NONE',  ( -1.000000000000000000, -0.000000000000000000, -0.000000000000000000 ) ) ;
#820 = EDGE_CURVE ( 'NONE', #7631, #6575, #13600, .T. ) ;
#821 = CARTESIAN_POINT ( 'NONE',  ( -2.943691928843435779, -14.79893867722909917, -15.50201066848093312 ) ) ;
#822 = DIRECTION ( 'NONE',  ( -1.000000000000000000, 0.000000000000000000, 0.000000000000000000 ) ) ;
#823 = ORIENTED_EDGE ( 'NONE', *, *, #14598, .T. ) ;
#824 = EDGE_CURVE ( 'NONE', #19846, #5684, #5131, .T. ) ;
#825 = CARTESIAN_POINT ( 'NONE',  ( 2.500000000000000000, -1.178949249685214307, 2.042000000000001592 ) ) ;
#826 = DIRECTION ( 'NONE',  ( -1.000000000000000000, 0.000000000000000000, 0.000000000000000000 ) ) ;
#827 = AXIS2_PLACEMENT_3D ( 'NONE', #10753, #14041, #6069 ) ;
#828 = ORIENTED_EDGE ( 'NONE', *, *, #1732, .T. ) ;
#829 = CARTESIAN_POINT ( 'NONE',  ( 1.577030005767653176, -22.95872380089934950, -75.39090623211717457 ) ) ;
#830 = ORIENTED_EDGE ( 'NONE', *, *, #2623, .F. ) ;
#831 = DIRECTION ( 'NONE',  ( -0.000000000000000000, -0.000000000000000000, 1.000000000000000000 ) ) ;
#832 = CARTESIAN_POINT ( 'NONE',  ( -15.25966316918061416, 10.19618095414378445, 8.150043750180310909 ) ) ;
#833 = VERTEX_POINT ( 'NONE', #18577 ) ;
#834 = VERTEX_POINT ( 'NONE', #15705 ) ;
#835 = DIRECTION ( 'NONE',  ( -1.000000000000000000, -0.000000000000000000, 0.000000000000000000 ) ) ;
#836 = VECTOR ( 'NONE', #4368, 1000.000000000000000 ) ;
#837 = FACE_BOUND ( 'NONE', #113, .T. ) ;
#838 = DIRECTION ( 'NONE',  ( -1.000000000000000000, -0.000000000000000000, -0.000000000000000000 ) ) ;
#839 = LINE ( 'NONE', #10479, #15988 ) ;
#840 = CARTESIAN_POINT ( 'NONE',  ( -18.00000000043041481, -3.580422610670022987, 18.30151875018031049 ) ) ;
#841 = CYLINDRICAL_SURFACE ( 'NONE', #7833, 27.60000000002760245 ) ;
#842 = CARTESIAN_POINT ( 'NONE',  ( -6.358192987158596488, 4.248408730893249441, -6.615206249819684636 ) ) ;
#843 = PRESENTATION_LAYER_ASSIGNMENT (  '', '', ( #10021 ) ) ;
#844 = CARTESIAN_POINT ( 'NONE',  ( 30.00000000000000000, -99.99999999999998579, -49.90000000000000568 ) ) ;
#845 = CARTESIAN_POINT ( 'NONE',  ( -11.17563879731704723, 1.343452237168308679E-09, -14.19260975028680605 ) ) ;
#846 = CARTESIAN_POINT ( 'NONE',  ( 9.999999999999998224, -36.59093685910587368, -62.00889726308067651 ) ) ;
#847 = MECHANICAL_DESIGN_GEOMETRIC_PRESENTATION_REPRESENTATION (  '', ( #8628 ), #6260 ) ;
#848 = ORIENTED_EDGE ( 'NONE', *, *, #778, .T. ) ;
#849 = DIRECTION ( 'NONE',  ( -0.000000000000000000, -0.000000000000000000, -1.000000000000000000 ) ) ;
#850 = CARTESIAN_POINT ( 'NONE',  ( 6.888301780572507305, -16.62983158603121936, -3.199262499819687022 ) ) ;
#851 = CARTESIAN_POINT ( 'NONE',  ( 9.999999999999998224, -67.51707036274397922, -25.00890260772446894 ) ) ;
#852 = ORIENTED_EDGE ( 'NONE', *, *, #20744, .T. ) ;
#853 = CARTESIAN_POINT ( 'NONE',  ( 85.00002539999999840, 0.000000000000000000, 0.000000000000000000 ) ) ;
#854 = EDGE_LOOP ( 'NONE', ( #53, #3141, #1269, #10123 ) ) ;
#855 = DIRECTION ( 'NONE',  ( 0.000000000000000000, -1.000000000000000000, 0.000000000000000000 ) ) ;
#856 = FACE_BOUND ( 'NONE', #9647, .T. ) ;
#857 = VERTEX_POINT ( 'NONE', #10629 ) ;
#858 = ORIENTED_EDGE ( 'NONE', *, *, #9285, .F. ) ;
#859 = CIRCLE ( 'NONE', #9469, 65.24900000006526568 ) ;
#860 = DIRECTION ( 'NONE',  ( -1.000000000000000000, 0.000000000000000000, 0.000000000000000000 ) ) ;
#861 = EDGE_CURVE ( 'NONE', #20459, #14616, #12427, .T. ) ;
#862 = CARTESIAN_POINT ( 'NONE',  ( -10.00000000000000000, 0.000000000000000000, 0.000000000000000000 ) ) ;
#863 = AXIS2_PLACEMENT_3D ( 'NONE', #4172, #11904, #3847 ) ;
#864 = LINE ( 'NONE', #6900, #20781 ) ;
#865 =( BOUNDED_CURVE ( )  B_SPLINE_CURVE ( 2, ( #12666, #20912, #11071, #7989, #4705, #3322, #4802, #6485, #17545, #11268, #15930, #11166, #17945, #34, #9684, #9572, #19426 ),
 .UNSPECIFIED., .F., .F. ) 
 B_SPLINE_CURVE_WITH_KNOTS ( ( 3, 2, 2, 2, 2, 2, 2, 2, 3 ),
 ( 0.5000000000038511416, 0.5125000000038510972, 0.5250000000038511638, 0.5375000000038511194, 0.5500000000038511860, 0.5625000000038511416, 0.5750000000038510972, 0.5875000000038511638, 0.6000000000038511194 ),
 .UNSPECIFIED. ) 
 CURVE ( )  GEOMETRIC_REPRESENTATION_ITEM ( )  RATIONAL_B_SPLINE_CURVE ( ( 0.9999999999940800688, 0.9807852804091503618, 1.000000000000000000, 0.9807852804032304306, 1.000000000000000000, 0.9807852804032304306, 1.000000000000000000, 0.9807852804032304306, 1.000000000000000000, 0.9807852804032304306, 1.000000000000000000, 0.9807852804032304306, 1.000000000000000000, 0.9807852804032304306, 1.000000000000000000, 0.9807852803973104994, 1.000000000005919931 ) ) 
 REPRESENTATION_ITEM ( '' )  );
#866 = CARTESIAN_POINT ( 'NONE',  ( 7.499999999820660790, -1.491842756249031954, -8.756668749819690234 ) ) ;
#867 = DIRECTION ( 'NONE',  ( -1.000000000000000000, 0.000000000000000000, 0.000000000000000000 ) ) ;
#868 = CYLINDRICAL_SURFACE ( 'NONE', #16265, 27.60000000002759890 ) ;
#869 = DIRECTION ( 'NONE',  ( 1.000000000000000000, 0.000000000000000000, 0.000000000000000000 ) ) ;
#870 = CARTESIAN_POINT ( 'NONE',  ( 0.000000000000000000, 8.857208570069802889, 71.45313048675089362 ) ) ;
#871 = EDGE_LOOP ( 'NONE', ( #2334, #11167, #13816, #14112, #20707, #13085 ) ) ;
#872 = DIRECTION ( 'NONE',  ( 0.000000000000000000, 0.000000000000000000, -1.000000000000000000 ) ) ;
#873 = CIRCLE ( 'NONE', #3566, 39.99999999999999289 ) ;
#874 = EDGE_LOOP ( 'NONE', ( #1892, #7772, #6301, #7238 ) ) ;
#875 = CARTESIAN_POINT ( 'NONE',  ( -10.19618095414378622, -15.25966316918061416, -3.631206249819686871 ) ) ;
#876 = CARTESIAN_POINT ( 'NONE',  ( 12.05832282520465704, -17.81513111787451464, 72.26823280878556943 ) ) ;
#877 =( REPRESENTATION_RELATIONSHIP ('NONE','NONE', #13739, #11016 ) REPRESENTATION_RELATIONSHIP_WITH_TRANSFORMATION ( #5360 )SHAPE_REPRESENTATION_RELATIONSHIP( ) );
#878 = EDGE_LOOP ( 'NONE', ( #15752, #1382 ) ) ;
#879 = CYLINDRICAL_SURFACE ( 'NONE', #19072, 72.00000000007199219 ) ;
#880 = VERTEX_POINT ( 'NONE', #4466 ) ;
#881 = VECTOR ( 'NONE', #12748, 1000.000000000000000 ) ;
#882 = FACE_OUTER_BOUND ( 'NONE', #5657, .T. ) ;
#883 = FACE_BOUND ( 'NONE', #8855, .T. ) ;
#884 = DIRECTION ( 'NONE',  ( -0.000000000000000000, -0.000000000000000000, 1.000000000000000000 ) ) ;
#885 = ORIENTED_EDGE ( 'NONE', *, *, #18800, .T. ) ;
#886 = DIRECTION ( 'NONE',  ( 1.000000000000000000, 0.000000000000000000, 0.000000000000000000 ) ) ;
#887 = ADVANCED_FACE ( 'NONE', ( #18899 ), #2880, .F. ) ;
#888 = CARTESIAN_POINT ( 'NONE',  ( 30.00000000000000355, -139.6410161513775563, 85.00000000000000000 ) ) ;
#889 = CARTESIAN_POINT ( 'NONE',  ( -10.19618095047497874, 15.25966317163202746, -0.6858937498196888694 ) ) ;
#890 = CARTESIAN_POINT ( 'NONE',  ( 0.000000000000000000, 0.000000000000000000, 46.00000000000000711 ) ) ;
#891 = MECHANICAL_DESIGN_GEOMETRIC_PRESENTATION_REPRESENTATION (  '', ( #4227 ), #19831 ) ;
#892 = CIRCLE ( 'NONE', #10354, 2.649999999999987477 ) ;
#893 = CARTESIAN_POINT ( 'NONE',  ( 19.99999999999999645, 0.000000000000000000, 0.000000000000000000 ) ) ;
#894 = CARTESIAN_POINT ( 'NONE',  ( 11.17563879758428769, 2.222972768810838939, -2.651921499352571931 ) ) ;
#895 = ADVANCED_FACE ( 'NONE', ( #10513 ), #7536, .T. ) ;
#896 = VERTEX_POINT ( 'NONE', #17088 ) ;
#897 = CIRCLE ( 'NONE', #7709, 27.60000000002759535 ) ;
#898 = TOROIDAL_SURFACE ( 'NONE', #13427, 2.700000000000000622, 0.2000000000000000111 ) ;
#899 = CYLINDRICAL_SURFACE ( 'NONE', #11693, 27.60000000002759890 ) ;
#900 = CARTESIAN_POINT ( 'NONE',  ( 10.00000000000000178, -164.9999999999999716, -70.00000000000000000 ) ) ;
#901 = ORIENTED_EDGE ( 'NONE', *, *, #12581, .T. ) ;
#902 = CARTESIAN_POINT ( 'NONE',  ( -13.32881486730456366, -16.88549087568889462, -72.74798471664084332 ) ) ;
#903 = EDGE_LOOP ( 'NONE', ( #239, #12883, #15311, #19138, #7059, #15330, #9122, #10048, #7226 ) ) ;
#904 = CARTESIAN_POINT ( 'NONE',  ( -18.00000000000000000, 2.163826221265758884E-09, -9.678949999819687733 ) ) ;
#905 = VECTOR ( 'NONE', #7979, 1000.000000000000000 ) ;
#906 = DIRECTION ( 'NONE',  ( -0.000000000000000000, -0.000000000000000000, 1.000000000000000000 ) ) ;
#907 = CARTESIAN_POINT ( 'NONE',  ( -15.14999999999999325, 3.245314017740474129E-16, 46.00000000000000711 ) ) ;
#908 = ORIENTED_EDGE ( 'NONE', *, *, #8321, .T. ) ;
#909 = LINE ( 'NONE', #7361, #12285 ) ;
#910 = AXIS2_PLACEMENT_3D ( 'NONE', #8362, #2107, #19388 ) ;
#911 = EDGE_LOOP ( 'NONE', ( #2651, #5379, #14973 ) ) ;
#912 = LINE ( 'NONE', #2704, #7153 ) ;
#913 = CIRCLE ( 'NONE', #2266, 0.2000000000000000944 ) ;
#914 = ORIENTED_EDGE ( 'NONE', *, *, #6745, .T. ) ;
#915 = CIRCLE ( 'NONE', #3928, 27.60000000002759535 ) ;
#916 = CARTESIAN_POINT ( 'NONE',  ( 30.00000000000000000, -105.0000000000000000, 72.35596062816881613 ) ) ;
#917 = ADVANCED_FACE ( 'NONE', ( #7647 ), #16971, .T. ) ;
#918 = DIRECTION ( 'NONE',  ( -1.000000000000000000, 0.000000000000000000, 0.000000000000000000 ) ) ;
#919 = APPLICATION_PROTOCOL_DEFINITION ( 'draft international standard', 'automotive_design', 1998, #17546 ) ;
#920 = VECTOR ( 'NONE', #7736, 1000.000000000000000 ) ;
#921 = CARTESIAN_POINT ( 'NONE',  ( -13.67243654778936168, -5.663308646854336992, 1.013729418841546437 ) ) ;
#922 = ADVANCED_FACE ( 'NONE', ( #4365 ), #2675, .F. ) ;
#923 = ORIENTED_EDGE ( 'NONE', *, *, #7287, .F. ) ;
#924 = AXIS2_PLACEMENT_3D ( 'NONE', #11112, #6114, #18854 ) ;
#925 = ADVANCED_FACE ( 'NONE', ( #12205 ), #9036, .T. ) ;
#926 = CARTESIAN_POINT ( 'NONE',  ( -4.000000000000000000, -2.309401076758531346, -5.242734410091827613 ) ) ;
#927 = ORIENTED_EDGE ( 'NONE', *, *, #11369, .F. ) ;
#928 = DIRECTION ( 'NONE',  ( 1.000000000000000000, 0.000000000000000000, 0.000000000000000000 ) ) ;
#929 = AXIS2_PLACEMENT_3D ( 'NONE', #67, #17673, #6521 ) ;
#930 = CARTESIAN_POINT ( 'NONE',  ( 15.25966316918061239, -10.19618095414378445, 3.437543750180311442 ) ) ;
#931 = AXIS2_PLACEMENT_3D ( 'NONE', #13991, #1176, #17274 ) ;
#932 = CARTESIAN_POINT ( 'NONE',  ( 0.000000000000000000, -28.84646472442495480, 58.52617768068423487 ) ) ;
#933 = DIRECTION ( 'NONE',  ( 0.000000000000000000, 0.000000000000000000, -1.000000000000000000 ) ) ;
#934 = EDGE_CURVE ( 'NONE', #273, #10935, #17300, .T. ) ;
#935 = EDGE_LOOP ( 'NONE', ( #17528, #12852, #4490, #10128 ) ) ;
#936 = LINE ( 'NONE', #1034, #3948 ) ;
#937 = PLANE ( 'NONE',  #1249 ) ;
#938 = VECTOR ( 'NONE', #2750, 1000.000000000000000 ) ;
#939 = VERTEX_POINT ( 'NONE', #17201 ) ;
#940 = CARTESIAN_POINT ( 'NONE',  ( 7.500000000000007105, -1.491842755816071175, 6.933231250087794173 ) ) ;
#941 = ORIENTED_EDGE ( 'NONE', *, *, #9394, .F. ) ;
#942 = CARTESIAN_POINT ( 'NONE',  ( 7.500000000000001776, -1.491842755816069843, 0.6683312500877865991 ) ) ;
#943 = CARTESIAN_POINT ( 'NONE',  ( 2.163825119083639120E-09, 17.99999999999999645, -18.65229999981968945 ) ) ;
#944 = B_SPLINE_CURVE_WITH_KNOTS ( 'NONE', 3,
 ( #16979, #3938, #20368, #5853, #573, #12328, #12116, #5424 ),
 .UNSPECIFIED., .F., .F.,
 ( 4, 2, 2, 4 ),
 ( 0.000000000000000000, 0.004496536736660343599, 0.006744805104990527975, 0.008993073473320711483 ),
 .UNSPECIFIED. ) ;
#945 = AXIS2_PLACEMENT_3D ( 'NONE', #809, #7256, #13736 ) ;
#946 = EDGE_LOOP ( 'NONE', ( #5356, #19237, #20255, #9417 ) ) ;
#947 = ORIENTED_EDGE ( 'NONE', *, *, #16251, .T. ) ;
#948 = CARTESIAN_POINT ( 'NONE',  ( 19.99999999999999645, -59.31169354540720207, -27.19476070466916795 ) ) ;
#949 = ADVANCED_FACE ( 'NONE', ( #1200 ), #13942, .T. ) ;
#950 = CARTESIAN_POINT ( 'NONE',  ( 0.000000000000000000, -58.26603306961992956, 42.29739224042451440 ) ) ;
#951 = CARTESIAN_POINT ( 'NONE',  ( 19.99999999999999645, 10.77748419466781726, -63.93680186330462334 ) ) ;
#952 = FACE_OUTER_BOUND ( 'NONE', #13338, .T. ) ;
#953 = CARTESIAN_POINT ( 'NONE',  ( 12.72792206288791128, 12.72792205982780267, 12.70542500018031085 ) ) ;
#954 = EDGE_CURVE ( 'NONE', #11144, #2302, #1092, .T. ) ;
#955 = UNCERTAINTY_MEASURE_WITH_UNIT (LENGTH_MEASURE( 1.000000000000000082E-05 ), #18012, 'distance_accuracy_value', 'NONE');
#956 = ADVANCED_FACE ( 'NONE', ( #9136 ), #20672, .T. ) ;
#957 = CARTESIAN_POINT ( 'NONE',  ( -21.18805271706017379, -3.649167310370820871, 90.00000000000000000 ) ) ;
#958 = CARTESIAN_POINT ( 'NONE',  ( 5.303300859536635770, 5.303300858261589923, 5.460575000180316607 ) ) ;
#959 = ORIENTED_EDGE ( 'NONE', *, *, #13129, .F. ) ;
#960 = DIRECTION ( 'NONE',  ( 0.000000000000000000, 0.000000000000000000, 1.000000000000000000 ) ) ;
#961 = CARTESIAN_POINT ( 'NONE',  ( -7.902369976724391343, 7.902369978624323110, -13.01448475028680285 ) ) ;
#962 = EDGE_CURVE ( 'NONE', #13763, #5564, #20472, .T. ) ;
#963 = CYLINDRICAL_SURFACE ( 'NONE', #14801, 4.000000000000000000 ) ;
#964 = VERTEX_POINT ( 'NONE', #3390 ) ;
#965 = DIRECTION ( 'NONE',  ( -1.000000000000000000, -0.000000000000000000, -0.000000000000000000 ) ) ;
#966 = DIRECTION ( 'NONE',  ( 1.000000000000000000, 0.000000000000000000, 0.000000000000000000 ) ) ;
#967 = DIRECTION ( 'NONE',  ( -0.000000000000000000, -0.000000000000000000, 1.000000000000000000 ) ) ;
#968 = ORIENTED_EDGE ( 'NONE', *, *, #17940, .F. ) ;
#969 = DIRECTION ( 'NONE',  ( 0.000000000000000000, 0.000000000000000000, 1.000000000000000000 ) ) ;
#970 = ORIENTED_EDGE ( 'NONE', *, *, #1090, .T. ) ;
#971 = DIRECTION ( 'NONE',  ( 1.000000000000000000, 0.000000000000000000, 0.000000000000000000 ) ) ;
#972 = DIRECTION ( 'NONE',  ( 1.000000000000000000, -0.000000000000000000, -0.000000000000000000 ) ) ;
#973 = ORIENTED_EDGE ( 'NONE', *, *, #11043, .T. ) ;
#974 = ORIENTED_EDGE ( 'NONE', *, *, #9877, .F. ) ;
#975 = CARTESIAN_POINT ( 'NONE',  ( -17.50000000000000355, 0.000000000000000000, 43.00000000000000000 ) ) ;
#976 = EDGE_CURVE ( 'NONE', #1075, #15567, #19684, .T. ) ;
#977 = DIRECTION ( 'NONE',  ( -1.000000000000000000, 0.000000000000000000, 0.000000000000000000 ) ) ;
#978 = EDGE_CURVE ( 'NONE', #11163, #4471, #17333, .T. ) ;
#979 = DIRECTION ( 'NONE',  ( 0.000000000000000000, 0.000000000000000000, 1.000000000000000000 ) ) ;
#980 = CARTESIAN_POINT ( 'NONE',  ( -4.248408729364575365, 6.358192988180014105, -2.866043749819687569 ) ) ;
#981 = SURFACE_STYLE_USAGE ( .BOTH. , #14017 ) ;
#982 = CARTESIAN_POINT ( 'NONE',  ( 41.41808208302013128, -123.1392381480534226, -87.79662768828312380 ) ) ;
#983 = DIRECTION ( 'NONE',  ( 1.000000000000000000, 0.000000000000000000, 0.000000000000000000 ) ) ;
#984 = DIRECTION ( 'NONE',  ( -1.000000000000000000, -0.000000000000000000, 0.000000000000000000 ) ) ;
#985 = ORIENTED_EDGE ( 'NONE', *, *, #409, .T. ) ;
#986 = EDGE_CURVE ( 'NONE', #3717, #7729, #20374, .T. ) ;
#987 = DIRECTION ( 'NONE',  ( -1.000000000000000000, -0.000000000000000000, -0.000000000000000000 ) ) ;
#988 = VERTEX_POINT ( 'NONE', #19106 ) ;
#989 = CARTESIAN_POINT ( 'NONE',  ( 12.72792205982779734, -12.72792206288791128, 3.732075000180311797 ) ) ;
#990 = CARTESIAN_POINT ( 'NONE',  ( 17.50000000000000355, 2.143131898507868643E-15, 46.00000000000000711 ) ) ;
#991 = ORIENTED_EDGE ( 'NONE', *, *, #19974, .T. ) ;
#992 = CARTESIAN_POINT ( 'NONE',  ( 85.00002539999999840, 0.000000000000000000, 1.000000000000000000 ) ) ;
#993 = ORIENTED_EDGE ( 'NONE', *, *, #14530, .T. ) ;
#994 = DIRECTION ( 'NONE',  ( -0.000000000000000000, -0.000000000000000000, -1.000000000000000000 ) ) ;
#995 = DIRECTION ( 'NONE',  ( 1.000000000000000000, 0.000000000000000000, -0.000000000000000000 ) ) ;
#996 = CARTESIAN_POINT ( 'NONE',  ( -24.99999999999999289, -1.326995226329868993, -84.99999999999998579 ) ) ;
#997 = ORIENTED_EDGE ( 'NONE', *, *, #9866, .T. ) ;
#998 = CARTESIAN_POINT ( 'NONE',  ( -1.491842756249033286, -7.499999999820668783, -18.98551874981968624 ) ) ;
#999 =( BOUNDED_CURVE ( )  B_SPLINE_CURVE ( 2, ( #12435, #18795, #1317, #19000, #10838, #9457, #6275, #7763, #12653, #3095, #17308, #2783, #7977, #14234, #7547, #20899, #2998 ),
 .UNSPECIFIED., .F., .T. ) 
 B_SPLINE_CURVE_WITH_KNOTS ( ( 3, 2, 2, 2, 2, 2, 2, 2, 3 ),
 ( 0.5000000000038511416, 0.5125000000038510972, 0.5250000000038511638, 0.5375000000038511194, 0.5500000000038511860, 0.5625000000038511416, 0.5750000000038510972, 0.5875000000038511638, 0.6000000000038511194 ),
 .UNSPECIFIED. ) 
 CURVE ( )  GEOMETRIC_REPRESENTATION_ITEM ( )  RATIONAL_B_SPLINE_CURVE ( ( 0.9999999999940800688, 0.9807852804091503618, 1.000000000000000000, 0.9807852804032304306, 1.000000000000000000, 0.9807852804032304306, 1.000000000000000000, 0.9807852804032304306, 1.000000000000000000, 0.9807852804032304306, 1.000000000000000000, 0.9807852804032304306, 1.000000000000000000, 0.9807852804032304306, 1.000000000000000000, 0.9807852803973104994, 1.000000000005919931 ) ) 
 REPRESENTATION_ITEM ( '' )  );
#1000 = DIRECTION ( 'NONE',  ( 0.000000000000000000, 0.000000000000000000, -1.000000000000000000 ) ) ;
#1001 = CARTESIAN_POINT ( 'NONE',  ( -62.49999999999999289, -40.00000000000000000, 0.000000000000000000 ) ) ;
#1002 = CARTESIAN_POINT ( 'NONE',  ( 19.99999999999999645, 0.000000000000000000, 0.000000000000000000 ) ) ;
#1003 = DIRECTION ( 'NONE',  ( 0.000000000000000000, 0.000000000000000000, 1.000000000000000000 ) ) ;
#1004 = ORIENTED_EDGE ( 'NONE', *, *, #9228, .F. ) ;
#1005 = CARTESIAN_POINT ( 'NONE',  ( -24.99999999999999289, -148.4917293642369600, 48.67032260359988527 ) ) ;
#1006 = ORIENTED_EDGE ( 'NONE', *, *, #7889, .T. ) ;
#1007 = CARTESIAN_POINT ( 'NONE',  ( 19.99999999999999645, 56.63599015375672963, 31.56633360682482703 ) ) ;
#1008 = CARTESIAN_POINT ( 'NONE',  ( -2.870125741905213079, 6.929096494179683319, -5.731612499819686235 ) ) ;
#1009 = EDGE_CURVE ( 'NONE', #14849, #19012, #17928, .T. ) ;
#1010 = EDGE_LOOP ( 'NONE', ( #1177, #17232, #20244, #6388 ) ) ;
#1011 = ADVANCED_FACE ( 'NONE', ( #9856 ), #8076, .T. ) ;
#1012 = CARTESIAN_POINT ( 'NONE',  ( 12.72792206288790950, 12.72792205982780089, -6.144574999819688799 ) ) ;
#1013 = CARTESIAN_POINT ( 'NONE',  ( 19.99999999999999645, -19.38316218894255627, 61.87375713200982119 ) ) ;
#1014 = PLANE ( 'NONE',  #4630 ) ;
#1015 = EDGE_LOOP ( 'NONE', ( #7142, #11524, #9589, #1232 ) ) ;
#1016 = DIRECTION ( 'NONE',  ( 0.000000000000000000, 0.000000000000000000, 1.000000000000000000 ) ) ;
#1017 = ORIENTED_EDGE ( 'NONE', *, *, #9002, .F. ) ;
#1018 = DIRECTION ( 'NONE',  ( 0.000000000000000000, 0.000000000000000000, 1.000000000000000000 ) ) ;
#1019 = ORIENTED_EDGE ( 'NONE', *, *, #7241, .F. ) ;
#1020 = AXIS2_PLACEMENT_3D ( 'NONE', #11935, #4312, #18410 ) ;
#1021 = CARTESIAN_POINT ( 'NONE',  ( -23.00000000000000000, 2.816687638038912352E-15, -130.0000000000000000 ) ) ;
#1022 = DIRECTION ( 'NONE',  ( 0.000000000000000000, 0.000000000000000000, 1.000000000000000000 ) ) ;
#1023 = ITEM_DEFINED_TRANSFORMATION ( 'NONE', 'NONE', #170,  #12461 ) ;
#1024 = ADVANCED_FACE ( 'NONE', ( #12950 ), #10, .T. ) ;
#1025 = CARTESIAN_POINT ( 'NONE',  ( 14.79893867793684059, 2.943691925285398359, 6.020760668841545815 ) ) ;
#1026 = EDGE_LOOP ( 'NONE', ( #11463, #10567, #20896 ) ) ;
#1027 = DIRECTION ( 'NONE',  ( -0.000000000000000000, 0.000000000000000000, -1.000000000000000000 ) ) ;
#1028 = ORIENTED_EDGE ( 'NONE', *, *, #9501, .F. ) ;
#1029 = LINE ( 'NONE', #7476, #16566 ) ;
#1030 = CARTESIAN_POINT ( 'NONE',  ( -2.163827323447877821E-09, -17.99999999999999645, 14.33520000018031126 ) ) ;
#1031 = DIRECTION ( 'NONE',  ( 0.000000000000000000, -0.4999999999999993339, 0.8660254037844390407 ) ) ;
#1032 = DIRECTION ( 'NONE',  ( 0.000000000000000000, 0.000000000000000000, 1.000000000000000000 ) ) ;
#1033 = ORIENTED_EDGE ( 'NONE', *, *, #9203, .T. ) ;
#1034 = CARTESIAN_POINT ( 'NONE',  ( 19.99999999999999645, -56.42118728228177105, 32.77318456705422278 ) ) ;
#1035 = CARTESIAN_POINT ( 'NONE',  ( 1.040949779275250179E-14, -85.00000000000000000, 19.00000000000000000 ) ) ;
#1036 = AXIS2_PLACEMENT_3D ( 'NONE', #5114, #5025, #13402 ) ;
#1037 = VERTEX_POINT ( 'NONE', #19402 ) ;
#1038 = ADVANCED_FACE ( 'NONE', ( #7857 ), #11357, .F. ) ;
#1039 = ADVANCED_FACE ( 'NONE', ( #3196 ), #1713, .T. ) ;
#1040 = CARTESIAN_POINT ( 'NONE',  ( 0.000000000000000000, -46.17500197033020015, -55.24372537266445704 ) ) ;
#1041 = DIRECTION ( 'NONE',  ( 1.000000000000000000, 1.836909530733573776E-16, 0.000000000000000000 ) ) ;
#1042 = CARTESIAN_POINT ( 'NONE',  ( -15.25966317163202923, -10.19618095047497874, -12.46714374981969264 ) ) ;
#1043 = ADVANCED_FACE ( 'NONE', ( #14443 ), #12752, .T. ) ;
#1044 = ORIENTED_EDGE ( 'NONE', *, *, #7397, .F. ) ;
#1045 = ORIENTED_EDGE ( 'NONE', *, *, #12467, .F. ) ;
#1046 = CARTESIAN_POINT ( 'NONE',  ( 6.249999999999902300, -10.82531754730554496, 46.00000000000000711 ) ) ;
#1047 = CARTESIAN_POINT ( 'NONE',  ( 0.000000000000000000, 38.22257254261821657, -61.01667762370101400 ) ) ;
#1048 = CONICAL_SURFACE ( 'NONE', #2397, 4.000000000000000000, 1.047197551196595855 ) ;
#1049 = DIRECTION ( 'NONE',  ( 1.000000000000000000, 0.000000000000000000, 0.000000000000000000 ) ) ;
#1050 = DIRECTION ( 'NONE',  ( 0.000000000000000000, 0.000000000000000000, 1.000000000000000000 ) ) ;
#1051 = SURFACE_STYLE_FILL_AREA ( #4103 ) ;
#1052 = CARTESIAN_POINT ( 'NONE',  ( 6.888301780572508193, -16.62983158603122291, -3.199262499819690575 ) ) ;
#1053 = ADVANCED_FACE ( 'NONE', ( #11041 ), #19206, .T. ) ;
#1054 = AXIS2_PLACEMENT_3D ( 'NONE', #7104, #2567, #13695 ) ;
#1055 = CARTESIAN_POINT ( 'NONE',  ( 4.000000000000003553, 2.309401076758524685, -0.3572655899081733644 ) ) ;
#1056 = ORIENTED_EDGE ( 'NONE', *, *, #693, .T. ) ;
#1057 = CARTESIAN_POINT ( 'NONE',  ( 52.00000000000000000, -99.99999999999998579, 5.000000000000000000 ) ) ;
#1058 = CARTESIAN_POINT ( 'NONE',  ( 14.79893867722909917, -2.943691928843437111, 10.41673933151907505 ) ) ;
#1059 = PRODUCT_DEFINITION_SHAPE ( 'NONE', 'NONE',  #20946 ) ;
#1060 = DIRECTION ( 'NONE',  ( 0.000000000000000000, 0.000000000000000000, -1.000000000000000000 ) ) ;
#1061 = VERTEX_POINT ( 'NONE', #17520 ) ;
#1062 = DIRECTION ( 'NONE',  ( 0.000000000000000000, 0.000000000000000000, -1.000000000000000000 ) ) ;
#1063 = CARTESIAN_POINT ( 'NONE',  ( -3.580422614997675002, -17.99999999956958163, -21.16566874981968738 ) ) ;
#1064 = CARTESIAN_POINT ( 'NONE',  ( 0.000000000000000000, 31.98952867950324830, 56.39803944231596944 ) ) ;
#1065 = EDGE_LOOP ( 'NONE', ( #17257, #14549, #3120, #18251 ) ) ;
#1066 = ADVANCED_FACE ( 'NONE', ( #20892 ), #9764, .F. ) ;
#1067 = DIRECTION ( 'NONE',  ( -1.000000000000000000, -0.000000000000000000, -0.000000000000000000 ) ) ;
#1068 = AXIS2_PLACEMENT_3D ( 'NONE', #11739, #18208, #9405 ) ;
#1069 = VERTEX_POINT ( 'NONE', #16020 ) ;
#1070 = DIRECTION ( 'NONE',  ( -1.000000000000000000, -0.000000000000000000, 0.000000000000000000 ) ) ;
#1071 = DIRECTION ( 'NONE',  ( 1.000000000000000000, 0.000000000000000000, 0.000000000000000000 ) ) ;
#1072 = ADVANCED_FACE ( 'NONE', ( #6572 ), #9550, .T. ) ;
#1073 = ORIENTED_EDGE ( 'NONE', *, *, #4313, .T. ) ;
#1074 = VECTOR ( 'NONE', #9967, 1000.000000000000000 ) ;
#1075 = VERTEX_POINT ( 'NONE', #2991 ) ;
#1076 = DIRECTION ( 'NONE',  ( -1.000000000000000000, -0.000000000000000000, -0.000000000000000000 ) ) ;
#1077 = EDGE_CURVE ( 'NONE', #1492, #12057, #9450, .T. ) ;
#1078 = AXIS2_PLACEMENT_3D ( 'NONE', #20638, #18751, #15770 ) ;
#1079 = DIRECTION ( 'NONE',  ( -1.000000000000000000, 0.000000000000000000, 0.000000000000000000 ) ) ;
#1080 = B_SPLINE_CURVE_WITH_KNOTS ( 'NONE', 3,
 ( #19450, #9709, #11496, #19760 ),
 .UNSPECIFIED., .F., .F.,
 ( 4, 4 ),
 ( 2.380737582495642427E-07, 0.002336974151641604130 ),
 .UNSPECIFIED. ) ;
#1081 = DIRECTION ( 'NONE',  ( 1.000000000000000000, 0.000000000000000000, 0.000000000000000000 ) ) ;
#1082 = AXIS2_PLACEMENT_3D ( 'NONE', #19195, #7847, #1081 ) ;
#1083 = AXIS2_PLACEMENT_3D ( 'NONE', #14869, #8398, #3931 ) ;
#1084 = CARTESIAN_POINT ( 'NONE',  ( -4.276731812588563386, 10.32494394809438987, 15.84957774971319822 ) ) ;
#1085 = DIRECTION ( 'NONE',  ( 0.000000000000000000, 0.000000000000000000, 1.000000000000000000 ) ) ;
#1086 = CIRCLE ( 'NONE', #9202, 10.79377999999999993 ) ;
#1087 = EDGE_CURVE ( 'NONE', #13160, #12463, #19294, .T. ) ;
#1088 = LINE ( 'NONE', #18896, #7048 ) ;
#1089 = DIRECTION ( 'NONE',  ( -1.000000000000000000, 0.000000000000000000, 0.000000000000000000 ) ) ;
#1090 = EDGE_CURVE ( 'NONE', #9449, #20554, #16633, .T. ) ;
#1091 = ORIENTED_EDGE ( 'NONE', *, *, #10308, .F. ) ;
#1092 = LINE ( 'NONE', #18992, #4812 ) ;
#1093 = ORIENTED_EDGE ( 'NONE', *, *, #16885, .F. ) ;
#1094 = CARTESIAN_POINT ( 'NONE',  ( 6.888301784570728614, 16.62983158437510056, -18.06323749981969229 ) ) ;
#1095 = CARTESIAN_POINT ( 'NONE',  ( 9.999999999999998224, 58.26603306961963824, 42.29739224042493362 ) ) ;
#1096 = CIRCLE ( 'NONE', #1020, 8.500000000000000000 ) ;
#1097 = ORIENTED_EDGE ( 'NONE', *, *, #18827, .T. ) ;
#1098 = CARTESIAN_POINT ( 'NONE',  ( 0.000000000000000000, 0.000000000000000000, 0.000000000000000000 ) ) ;
#1099 = VERTEX_POINT ( 'NONE', #18442 ) ;
#1100 = FACE_OUTER_BOUND ( 'NONE', #13056, .T. ) ;
#1101 = DIRECTION ( 'NONE',  ( 0.000000000000000000, 0.000000000000000000, 1.000000000000000000 ) ) ;
#1102 = DIRECTION ( 'NONE',  ( -1.000000000000000000, 0.000000000000000000, 0.000000000000000000 ) ) ;
#1103 = EDGE_CURVE ( 'NONE', #4018, #1536, #6170, .T. ) ;
#1104 = ORIENTED_EDGE ( 'NONE', *, *, #20743, .F. ) ;
#1105 = CARTESIAN_POINT ( 'NONE',  ( -24.99999999999999289, -85.00000000000000000, -1.040949779275250179E-14 ) ) ;
#1106 = AXIS2_PLACEMENT_3D ( 'NONE', #20639, #6117, #6226 ) ;
#1107 = VECTOR ( 'NONE', #1062, 1000.000000000000000 ) ;
#1108 = AXIS2_PLACEMENT_3D ( 'NONE', #14210, #12619, #4013 ) ;
#1109 = CYLINDRICAL_SURFACE ( 'NONE', #5621, 65.24900000006525147 ) ;
#1110 = CYLINDRICAL_SURFACE ( 'NONE', #14068, 10.00000000000000178 ) ;
#1111 = DIRECTION ( 'NONE',  ( 0.000000000000000000, 0.000000000000000000, 1.000000000000000000 ) ) ;
#1112 = FACE_OUTER_BOUND ( 'NONE', #19436, .T. ) ;
#1113 = ORIENTED_EDGE ( 'NONE', *, *, #20190, .F. ) ;
#1114 = DIRECTION ( 'NONE',  ( 0.000000000000000000, 0.000000000000000000, 1.000000000000000000 ) ) ;
#1115 = FACE_OUTER_BOUND ( 'NONE', #5139, .T. ) ;
#1116 = VERTEX_POINT ( 'NONE', #13564 ) ;
#1117 = AXIS2_PLACEMENT_3D ( 'NONE', #10896, #20640, #17584 ) ;
#1118 = CARTESIAN_POINT ( 'NONE',  ( 2.500000000000000000, 1.178949249685213863, -2.042000000000001148 ) ) ;
#1119 = LINE ( 'NONE', #20388, #2474 ) ;
#1120 = VECTOR ( 'NONE', #11332, 1000.000000000000000 ) ;
#1121 = ORIENTED_EDGE ( 'NONE', *, *, #14490, .T. ) ;
#1122 = AXIS2_PLACEMENT_3D ( 'NONE', #5465, #6955, #2193 ) ;
#1123 = CARTESIAN_POINT ( 'NONE',  ( -15.25966317163203279, -10.19618095047498052, -19.98754374981969306 ) ) ;
#1124 = VECTOR ( 'NONE', #2201, 1000.000000000000000 ) ;
#1125 = CARTESIAN_POINT ( 'NONE',  ( -65.00002539999999840, 0.000000000000000000, 0.000000000000000000 ) ) ;
#1126 = DIRECTION ( 'NONE',  ( -0.000000000000000000, -0.000000000000000000, 1.000000000000000000 ) ) ;
#1127 = VERTEX_POINT ( 'NONE', #13365 ) ;
#1128 = CARTESIAN_POINT ( 'NONE',  ( 19.99999999999999645, -8.857208570070305598, 71.45313048675082257 ) ) ;
#1129 = ORIENTED_EDGE ( 'NONE', *, *, #7364, .T. ) ;
#1130 = FACE_OUTER_BOUND ( 'NONE', #6284, .T. ) ;
#1131 = CIRCLE ( 'NONE', #2124, 7.500000000000000000 ) ;
#1132 = ORIENTED_EDGE ( 'NONE', *, *, #20108, .T. ) ;
#1133 = DIRECTION ( 'NONE',  ( 0.000000000000000000, 0.000000000000000000, -1.000000000000000000 ) ) ;
#1134 = EDGE_CURVE ( 'NONE', #14374, #16949, #2327, .T. ) ;
#1135 = LINE ( 'NONE', #15949, #12648 ) ;
#1136 = CARTESIAN_POINT ( 'NONE',  ( -5.663308646854337880, 13.67243654778935991, -6.055020581158455428 ) ) ;
#1137 = ORIENTED_EDGE ( 'NONE', *, *, #15695, .T. ) ;
#1138 = CARTESIAN_POINT ( 'NONE',  ( 0.000000000000000000, 0.000000000000000000, 0.000000000000000000 ) ) ;
#1139 = ORIENTED_EDGE ( 'NONE', *, *, #7007, .F. ) ;
#1140 = CIRCLE ( 'NONE', #15346, 21.50000000000000000 ) ;
#1141 = CARTESIAN_POINT ( 'NONE',  ( 4.248408729364576253, -6.358192988180015881, -26.42854374981969556 ) ) ;
#1142 = CIRCLE ( 'NONE', #12662, 65.24900000006525147 ) ;
#1143 = CARTESIAN_POINT ( 'NONE',  ( 2.163825119083639120E-09, 17.99999999999999645, 0.1977000001803091989 ) ) ;
#1144 = DIRECTION ( 'NONE',  ( -1.000000000000000000, 0.000000000000000000, 0.000000000000000000 ) ) ;
#1145 = LINE ( 'NONE', #18944, #6305 ) ;
#1146 = AXIS2_PLACEMENT_3D ( 'NONE', #18374, #13715, #7032 ) ;
#1147 = CIRCLE ( 'NONE', #8224, 72.00000000007199219 ) ;
#1148 = ORIENTED_EDGE ( 'NONE', *, *, #5311, .F. ) ;
#1149 = CARTESIAN_POINT ( 'NONE',  ( 30.00000000000000000, -85.00000000000000000, -1.040949779275250179E-14 ) ) ;
#1150 = LINE ( 'NONE', #10570, #2963 ) ;
#1151 = ORIENTED_EDGE ( 'NONE', *, *, #17537, .T. ) ;
#1152 = CARTESIAN_POINT ( 'NONE',  ( 0.000000000000000000, 0.000000000000000000, 0.000000000000000000 ) ) ;
#1153 = CARTESIAN_POINT ( 'NONE',  ( 6.359999999999997655, 7.000462221625649605E-15, 0.000000000000000000 ) ) ;
#1154 = CARTESIAN_POINT ( 'NONE',  ( 6.888301780572505528, -16.62983158603121581, -5.103862499819689980 ) ) ;
#1155 = VECTOR ( 'NONE', #3414, 1000.000000000000000 ) ;
#1156 = ORIENTED_EDGE ( 'NONE', *, *, #6424, .T. ) ;
#1157 = CARTESIAN_POINT ( 'NONE',  ( -6.358192988180021210, -4.248408729364580694, -8.382393749819687656 ) ) ;
#1158 = AXIS2_PLACEMENT_3D ( 'NONE', #9951, #6764, #14839 ) ;
#1159 = AXIS2_PLACEMENT_3D ( 'NONE', #14472, #7776, #9575 ) ;
#1160 = CARTESIAN_POINT ( 'NONE',  ( 0.000000000000000000, 0.000000000000000000, 0.000000000000000000 ) ) ;
#1161 = EDGE_CURVE ( 'NONE', #7789, #5332, #14980, .T. ) ;
#1162 = CARTESIAN_POINT ( 'NONE',  ( 0.000000000000000000, 36.54710069451054011, 54.05313526368126276 ) ) ;
#1163 = DIRECTION ( 'NONE',  ( -1.000000000000000000, -0.000000000000000000, -0.000000000000000000 ) ) ;
#1164 = DIRECTION ( 'NONE',  ( 0.000000000000000000, 0.4484107612694736567, 0.8938276059608648572 ) ) ;
#1165 = CARTESIAN_POINT ( 'NONE',  ( -16.62983158437510411, 6.888301784570731279, 0.3351125001803089143 ) ) ;
#1166 = AXIS2_PLACEMENT_3D ( 'NONE', #9873, #14559, #8482 ) ;
#1167 = AXIS2_PLACEMENT_3D ( 'NONE', #15816, #15501, #12651 ) ;
#1168 = CIRCLE ( 'NONE', #13352, 2.649999999999999467 ) ;
#1169 = CARTESIAN_POINT ( 'NONE',  ( -6.929096493489632635, 2.870125743571140919, -16.33473749981968837 ) ) ;
#1170 =( REPRESENTATION_RELATIONSHIP ('NONE','NONE', #13739, #11016 ) REPRESENTATION_RELATIONSHIP_WITH_TRANSFORMATION ( #3756 )SHAPE_REPRESENTATION_RELATIONSHIP( ) );
#1171 = ORIENTED_EDGE ( 'NONE', *, *, #13628, .F. ) ;
#1172 = DIRECTION ( 'NONE',  ( -1.000000000000000000, -0.000000000000000000, 0.000000000000000000 ) ) ;
#1173 = EDGE_CURVE ( 'NONE', #2494, #7434, #1775, .T. ) ;
#1174 = CARTESIAN_POINT ( 'NONE',  ( 13.67243654778934925, 5.663308646854335215, 18.95814558151907647 ) ) ;
#1175 = AXIS2_PLACEMENT_3D ( 'NONE', #13507, #18591, #15511 ) ;
#1176 = DIRECTION ( 'NONE',  ( -2.249565377136137858E-32, 1.224646799147353207E-16, 1.000000000000000000 ) ) ;
#1177 = ORIENTED_EDGE ( 'NONE', *, *, #15640, .F. ) ;
#1178 = LINE ( 'NONE', #7406, #18347 ) ;
#1179 = PLANE ( 'NONE',  #12072 ) ;
#1180 = DIRECTION ( 'NONE',  ( 0.000000000000000000, 0.000000000000000000, -1.000000000000000000 ) ) ;
#1181 = AXIS2_PLACEMENT_3D ( 'NONE', #6590, #9881, #17748 ) ;
#1182 = VERTEX_POINT ( 'NONE', #11768 ) ;
#1183 = FACE_OUTER_BOUND ( 'NONE', #6325, .T. ) ;
#1184 = ORIENTED_EDGE ( 'NONE', *, *, #15598, .T. ) ;
#1185 = VECTOR ( 'NONE', #19710, 1000.000000000000000 ) ;
#1186 = CARTESIAN_POINT ( 'NONE',  ( 32.16538072331778864, -33.51036596020169611, -72.20447320033530048 ) ) ;
#1187 = DIRECTION ( 'NONE',  ( 1.000000000000000000, 0.000000000000000000, 0.000000000000000000 ) ) ;
#1188 = ORIENTED_EDGE ( 'NONE', *, *, #8973, .T. ) ;
#1189 = VERTEX_POINT ( 'NONE', #3697 ) ;
#1190 = DIRECTION ( 'NONE',  ( -0.000000000000000000, -0.000000000000000000, 1.000000000000000000 ) ) ;
#1191 = LINE ( 'NONE', #20570, #20758 ) ;
#1192 = CYLINDRICAL_SURFACE ( 'NONE', #2080, 18.00000000000000000 ) ;
#1193 = EDGE_CURVE ( 'NONE', #10244, #7176, #5295, .T. ) ;
#1194 = CARTESIAN_POINT ( 'NONE',  ( -2.222972768810836275, 11.17563879758427525, 16.14410899971320035 ) ) ;
#1195 = ADVANCED_FACE ( 'NONE', ( #10170 ), #2017, .T. ) ;
#1196 = FILL_AREA_STYLE ('',( #10623 ) ) ;
#1197 = CARTESIAN_POINT ( 'NONE',  ( 0.000000000000000000, 0.000000000000000000, -90.00000000000000000 ) ) ;
#1198 = DIRECTION ( 'NONE',  ( 0.000000000000000000, 0.000000000000000000, -1.000000000000000000 ) ) ;
#1199 = ORIENTED_EDGE ( 'NONE', *, *, #18611, .F. ) ;
#1200 = FACE_OUTER_BOUND ( 'NONE', #19189, .T. ) ;
#1201 = ORIENTED_EDGE ( 'NONE', *, *, #13871, .T. ) ;
#1202 = EDGE_CURVE ( 'NONE', #20933, #12828, #18015, .T. ) ;
#1203 = CARTESIAN_POINT ( 'NONE',  ( -3.580422614997675002, -17.99999999956958163, -23.07026874981968945 ) ) ;
#1204 = CARTESIAN_POINT ( 'NONE',  ( 0.000000000000000000, 0.000000000000000000, 0.000000000000000000 ) ) ;
#1205 = EDGE_CURVE ( 'NONE', #6855, #6330, #4480, .T. ) ;
#1206 = AXIS2_PLACEMENT_3D ( 'NONE', #6335, #9204, #14298 ) ;
#1207 = ORIENTED_EDGE ( 'NONE', *, *, #18193, .F. ) ;
#1208 = DIRECTION ( 'NONE',  ( 0.000000000000000000, 0.000000000000000000, 1.000000000000000000 ) ) ;
#1209 = ORIENTED_EDGE ( 'NONE', *, *, #12607, .T. ) ;
#1210 = CYLINDRICAL_SURFACE ( 'NONE', #17638, 17.50000000000000355 ) ;
#1211 = CARTESIAN_POINT ( 'NONE',  ( -25.00000000000000000, -30.00000000000000711, 58.09475019311124555 ) ) ;
#1212 = CARTESIAN_POINT ( 'NONE',  ( 7.500000000000002665, 1.491842754878804689, 0.07926875008778555554 ) ) ;
#1213 = VERTEX_POINT ( 'NONE', #19915 ) ;
#1214 = DIRECTION ( 'NONE',  ( 1.000000000000000000, -0.000000000000000000, -0.000000000000000000 ) ) ;
#1215 = AXIS2_PLACEMENT_3D ( 'NONE', #14046, #12549, #3215 ) ;
#1216 = CARTESIAN_POINT ( 'NONE',  ( -12.50000000000000533, 0.000000000000000000, -43.00000000000000000 ) ) ;
#1217 = LINE ( 'NONE', #7663, #17114 ) ;
#1218 = CARTESIAN_POINT ( 'NONE',  ( -31.75000000000000000, 0.000000000000000000, 0.000000000000000000 ) ) ;
#1219 = EDGE_CURVE ( 'NONE', #4158, #16611, #3452, .T. ) ;
#1220 = CARTESIAN_POINT ( 'NONE',  ( 0.000000000000000000, 0.000000000000000000, 0.000000000000000000 ) ) ;
#1221 = ORIENTED_EDGE ( 'NONE', *, *, #7003, .T. ) ;
#1222 = EDGE_CURVE ( 'NONE', #12434, #19457, #19607, .T. ) ;
#1223 = DIRECTION ( 'NONE',  ( 0.000000000000000000, -1.224646799147354686E-16, 1.000000000000000000 ) ) ;
#1224 = VECTOR ( 'NONE', #20821, 1000.000000000000000 ) ;
#1225 = ADVANCED_FACE ( 'NONE', ( #8466, #5493 ), #3798, .F. ) ;
#1226 = DIRECTION ( 'NONE',  ( -1.000000000000000000, -0.000000000000000000, -0.000000000000000000 ) ) ;
#1227 = VERTEX_POINT ( 'NONE', #3598 ) ;
#1228 = CARTESIAN_POINT ( 'NONE',  ( 30.00000000000000000, -30.00000000000000711, -50.99019513592786268 ) ) ;
#1229 = CARTESIAN_POINT ( 'NONE',  ( 19.99999999999999645, 56.42118728228154367, 32.77318456705460648 ) ) ;
#1230 = VECTOR ( 'NONE', #984, 1000.000000000000000 ) ;
#1231 = ADVANCED_FACE ( 'NONE', ( #6774 ), #15157, .T. ) ;
#1232 = ORIENTED_EDGE ( 'NONE', *, *, #1161, .T. ) ;
#1233 = CARTESIAN_POINT ( 'NONE',  ( -3.580422614997675002, -17.99999999956958163, -11.74066874981969200 ) ) ;
#1234 = DIRECTION ( 'NONE',  ( 0.000000000000000000, 0.000000000000000000, -1.000000000000000000 ) ) ;
#1235 = CARTESIAN_POINT ( 'NONE',  ( 6.250000000000054179, 10.82531754730546147, 46.00000000000000711 ) ) ;
#1236 = ORIENTED_EDGE ( 'NONE', *, *, #16218, .F. ) ;
#1237 = CARTESIAN_POINT ( 'NONE',  ( 19.99999999999999645, -56.42118728228177105, 32.77318456705422278 ) ) ;
#1238 = EDGE_LOOP ( 'NONE', ( #176, #20104, #6054, #11712 ) ) ;
#1239 = DIRECTION ( 'NONE',  ( -0.000000000000000000, 0.000000000000000000, 1.000000000000000000 ) ) ;
#1240 = EDGE_LOOP ( 'NONE', ( #13575, #8868, #19150, #7093 ) ) ;
#1241 = AXIS2_PLACEMENT_3D ( 'NONE', #11873, #5718, #10613 ) ;
#1242 = CARTESIAN_POINT ( 'NONE',  ( 33.96219957007294710, -116.9571213503516987, 76.69693868221141031 ) ) ;
#1243 = EDGE_CURVE ( 'NONE', #5717, #20215, #4131, .T. ) ;
#1244 = AXIS2_PLACEMENT_3D ( 'NONE', #4937, #17777, #277 ) ;
#1245 = DIRECTION ( 'NONE',  ( 0.000000000000000000, 0.000000000000000000, -1.000000000000000000 ) ) ;
#1246 = CONTEXT_DEPENDENT_SHAPE_REPRESENTATION ( #9536, #9005 ) ;
#1247 = CARTESIAN_POINT ( 'NONE',  ( -5.663308650141539502, -13.67243654642775574, -9.589395581158459692 ) ) ;
#1248 = ORIENTED_EDGE ( 'NONE', *, *, #19286, .F. ) ;
#1249 = AXIS2_PLACEMENT_3D ( 'NONE', #17251, #13857, #4209 ) ;
#1250 = CARTESIAN_POINT ( 'NONE',  ( -10.00000000000000000, 0.000000000000000000, 0.000000000000000000 ) ) ;
#1251 = ORIENTED_EDGE ( 'NONE', *, *, #20171, .F. ) ;
#1252 = CARTESIAN_POINT ( 'NONE',  ( 10.80938043796751558, -18.58836422458828608, 77.51093294648217125 ) ) ;
#1253 = AXIS2_PLACEMENT_3D ( 'NONE', #309, #11755, #18221 ) ;
#1254 = CARTESIAN_POINT ( 'NONE',  ( 15.25966316918061239, -10.19618095414378445, 12.86254375018030949 ) ) ;
#1255 = AXIS2_PLACEMENT_3D ( 'NONE', #12708, #4424, #4330 ) ;
#1256 = CARTESIAN_POINT ( 'NONE',  ( -5.303300858261584594, 5.303300859536631329, -22.01057499981969556 ) ) ;
#1257 = CYLINDRICAL_SURFACE ( 'NONE', #17485, 72.00000000007199219 ) ;
#1258 = CIRCLE ( 'NONE', #6320, 65.24900000006525147 ) ;
#1259 = VECTOR ( 'NONE', #13520, 1000.000000000000000 ) ;
#1260 = ORIENTED_EDGE ( 'NONE', *, *, #1340, .F. ) ;
#1261 = EDGE_CURVE ( 'NONE', #9697, #4217, #5473, .T. ) ;
#1262 = LINE ( 'NONE', #15866, #6665 ) ;
#1263 = DIRECTION ( 'NONE',  ( -1.000000000000000000, -0.000000000000000000, -0.000000000000000000 ) ) ;
#1264 = ORIENTED_EDGE ( 'NONE', *, *, #19475, .F. ) ;
#1265 = CARTESIAN_POINT ( 'NONE',  ( -22.70866746290765903, -3.649167310370807105, -90.00000000000000000 ) ) ;
#1266 = CARTESIAN_POINT ( 'NONE',  ( 40.00000000000000711, 29.99999999999999289, -120.0000000000000142 ) ) ;
#1267 = CARTESIAN_POINT ( 'NONE',  ( -10.19618095047497874, 15.25966317163202746, -19.53589374981969229 ) ) ;
#1268 = CIRCLE ( 'NONE', #18495, 27.60000000002759890 ) ;
#1269 = ORIENTED_EDGE ( 'NONE', *, *, #18258, .T. ) ;
#1270 = DIRECTION ( 'NONE',  ( -1.000000000000000000, -0.000000000000000000, 0.000000000000000000 ) ) ;
#1271 = DIRECTION ( 'NONE',  ( 0.000000000000000000, 0.000000000000000000, 1.000000000000000000 ) ) ;
#1272 = CIRCLE ( 'NONE', #19871, 2.649999999999988365 ) ;
#1273 = CYLINDRICAL_SURFACE ( 'NONE', #6149, 21.50000000000000000 ) ;
#1274 = CARTESIAN_POINT ( 'NONE',  ( 50.00000000000000000, 31.35083268962918979, -84.99999999999998579 ) ) ;
#1275 = CARTESIAN_POINT ( 'NONE',  ( -12.50000000000000888, 1.700029006457270953E-13, 34.39999999999999858 ) ) ;
#1276 = CARTESIAN_POINT ( 'NONE',  ( -6.888301784570739272, -16.62983158437509701, -2.021137499819691818 ) ) ;
#1277 = VECTOR ( 'NONE', #14393, 1000.000000000000000 ) ;
#1278 = AXIS2_PLACEMENT_3D ( 'NONE', #13562, #5291, #10487 ) ;
#1279 = DIRECTION ( 'NONE',  ( 1.000000000000000000, 1.836909530733573776E-16, 0.000000000000000000 ) ) ;
#1280 = ORIENTED_EDGE ( 'NONE', *, *, #6566, .T. ) ;
#1281 = DIRECTION ( 'NONE',  ( 1.000000000000000000, 0.000000000000000000, 0.000000000000000000 ) ) ;
#1282 = CARTESIAN_POINT ( 'NONE',  ( -5.663308646854335215, 13.67243654778934925, 7.176895581519076472 ) ) ;
#1283 = VECTOR ( 'NONE', #512, 1000.000000000000000 ) ;
#1284 = ORIENTED_EDGE ( 'NONE', *, *, #1358, .T. ) ;
#1285 = ADVANCED_FACE ( 'NONE', ( #16853 ), #219, .F. ) ;
#1286 = CARTESIAN_POINT ( 'NONE',  ( 30.00000000000000000, -99.99999999999998579, -49.89999999999999858 ) ) ;
#1287 = AXIS2_PLACEMENT_3D ( 'NONE', #1447, #15948, #11287 ) ;
#1288 = DIRECTION ( 'NONE',  ( 0.000000000000000000, 0.000000000000000000, -1.000000000000000000 ) ) ;
#1289 = CARTESIAN_POINT ( 'NONE',  ( -44.00000000000000000, -85.00000000000000000, -1.040949779275250179E-14 ) ) ;
#1290 = EDGE_LOOP ( 'NONE', ( #10169, #20048, #12447, #7217 ) ) ;
#1291 = DIRECTION ( 'NONE',  ( -1.000000000000000000, -0.000000000000000000, 0.000000000000000000 ) ) ;
#1292 = CIRCLE ( 'NONE', #2284, 72.00000000007199219 ) ;
#1293 = ORIENTED_EDGE ( 'NONE', *, *, #10415, .F. ) ;
#1294 = CARTESIAN_POINT ( 'NONE',  ( 0.000000000000000000, -70.68211945903199478, 13.71269443944184196 ) ) ;
#1295 = FACE_OUTER_BOUND ( 'NONE', #6113, .T. ) ;
#1296 = AXIS2_PLACEMENT_3D ( 'NONE', #9806, #16273, #1763 ) ;
#1297 = ORIENTED_EDGE ( 'NONE', *, *, #3568, .T. ) ;
#1298 = VERTEX_POINT ( 'NONE', #9008 ) ;
#1299 = DIRECTION ( 'NONE',  ( -1.000000000000000000, 0.000000000000000000, 0.000000000000000000 ) ) ;
#1300 =( REPRESENTATION_RELATIONSHIP ('NONE','NONE', #13739, #4392 ) REPRESENTATION_RELATIONSHIP_WITH_TRANSFORMATION ( #15217 )SHAPE_REPRESENTATION_RELATIONSHIP( ) );
#1301 = VECTOR ( 'NONE', #16668, 1000.000000000000000 ) ;
#1302 = CARTESIAN_POINT ( 'NONE',  ( -12.50000000000000533, 0.000000000000000000, 166.0000000000000000 ) ) ;
#1303 = VECTOR ( 'NONE', #20268, 1000.000000000000000 ) ;
#1304 = DIRECTION ( 'NONE',  ( -1.000000000000000000, 0.000000000000000000, -0.000000000000000000 ) ) ;
#1305 = CARTESIAN_POINT ( 'NONE',  ( 4.276731812588570492, -10.32494394809439697, -0.5902027493525709989 ) ) ;
#1306 = CARTESIAN_POINT ( 'NONE',  ( 1.491842754445842134, -7.500000000179339210, -25.83948124981969130 ) ) ;
#1307 = CARTESIAN_POINT ( 'NONE',  ( -30.00000000000000000, -105.0000000000000426, 77.45966692414833688 ) ) ;
#1308 = CARTESIAN_POINT ( 'NONE',  ( 2.500000000000000000, 1.178949249685218525, 2.041999999999999371 ) ) ;
#1309 = EDGE_LOOP ( 'NONE', ( #5582, #5255, #19087, #7565 ) ) ;
#1310 = DIRECTION ( 'NONE',  ( 0.000000000000000000, 0.000000000000000000, -1.000000000000000000 ) ) ;
#1311 = ORIENTED_EDGE ( 'NONE', *, *, #1323, .F. ) ;
#1312 = CARTESIAN_POINT ( 'NONE',  ( 17.99999999956958163, -3.580422614997676334, -6.576518749819688203 ) ) ;
#1313 = CARTESIAN_POINT ( 'NONE',  ( 20.90734068544160706, -5.044436930659520257, 81.16927884214385358 ) ) ;
#1314 = ORIENTED_EDGE ( 'NONE', *, *, #11453, .F. ) ;
#1315 = LINE ( 'NONE', #992, #18069 ) ;
#1316 = VERTEX_POINT ( 'NONE', #13884 ) ;
#1317 = CARTESIAN_POINT ( 'NONE',  ( -6.929096494179678878, -2.870125741905209971, -4.927762499819690944 ) ) ;
#1318 = PLANE ( 'NONE',  #3965 ) ;
#1319 = DIRECTION ( 'NONE',  ( -1.000000000000000000, -0.000000000000000000, -0.000000000000000000 ) ) ;
#1320 = VERTEX_POINT ( 'NONE', #20123 ) ;
#1321 = DIRECTION ( 'NONE',  ( -1.000000000000000000, -0.000000000000000000, 0.000000000000000000 ) ) ;
#1322 = EDGE_CURVE ( 'NONE', #1127, #14263, #3129, .T. ) ;
#1323 = EDGE_CURVE ( 'NONE', #20518, #9271, #20328, .T. ) ;
#1324 = PLANE ( 'NONE',  #12771 ) ;
#1325 = CARTESIAN_POINT ( 'NONE',  ( 2.500000000000000000, 1.178949249685212974, -2.042000000000001148 ) ) ;
#1326 = DIRECTION ( 'NONE',  ( 1.000000000000000000, 1.836909530733573776E-16, 0.000000000000000000 ) ) ;
#1327 = DIRECTION ( 'NONE',  ( 0.000000000000000000, 0.000000000000000000, 1.000000000000000000 ) ) ;
#1328 = EDGE_CURVE ( 'NONE', #10217, #3338, #17694, .T. ) ;
#1329 = ORIENTED_EDGE ( 'NONE', *, *, #17632, .F. ) ;
#1330 = DIRECTION ( 'NONE',  ( 1.000000000000000000, -0.000000000000000000, 0.000000000000000000 ) ) ;
#1331 = DIRECTION ( 'NONE',  ( 0.000000000000000000, 0.000000000000000000, 1.000000000000000000 ) ) ;
#1332 = VERTEX_POINT ( 'NONE', #9114 ) ;
#1333 = CARTESIAN_POINT ( 'NONE',  ( 40.00000000000000711, -40.00000000000001421, -120.0000000000000142 ) ) ;
#1334 = CARTESIAN_POINT ( 'NONE',  ( -6.232800000000000118, 10.79377999999999993, 0.000000000000000000 ) ) ;
#1335 = ORIENTED_EDGE ( 'NONE', *, *, #13765, .F. ) ;
#1336 = CARTESIAN_POINT ( 'NONE',  ( 17.99999999956958163, -3.580422614997676334, -4.671918749819689687 ) ) ;
#1337 = PLANE ( 'NONE',  #3265 ) ;
#1338 = FACE_OUTER_BOUND ( 'NONE', #19789, .T. ) ;
#1339 = ORIENTED_EDGE ( 'NONE', *, *, #16121, .F. ) ;
#1340 = EDGE_CURVE ( 'NONE', #7434, #17615, #18406, .T. ) ;
#1341 = CARTESIAN_POINT ( 'NONE',  ( 19.99999999999999645, -63.05226888949902531, 15.11556105343437828 ) ) ;
#1342 = ORIENTED_EDGE ( 'NONE', *, *, #18173, .T. ) ;
#1343 = DIRECTION ( 'NONE',  ( -1.000000000000000000, 0.000000000000000000, 0.000000000000000000 ) ) ;
#1344 = ORIENTED_EDGE ( 'NONE', *, *, #20119, .T. ) ;
#1345 = EDGE_CURVE ( 'NONE', #15776, #2254, #12179, .T. ) ;
#1346 = EDGE_CURVE ( 'NONE', #14024, #6043, #20389, .T. ) ;
#1347 = AXIS2_PLACEMENT_3D ( 'NONE', #17925, #4887, #11354 ) ;
#1348 = EDGE_CURVE ( 'NONE', #4487, #10714, #7190, .T. ) ;
#1349 = CARTESIAN_POINT ( 'NONE',  ( 5.200000000000002842, 0.000000000000000000, 0.000000000000000000 ) ) ;
#1350 = CARTESIAN_POINT ( 'NONE',  ( -14.79893867722910628, 2.943691928843437111, 1.897323168841544394 ) ) ;
#1351 = ORIENTED_EDGE ( 'NONE', *, *, #8849, .T. ) ;
#1352 = CARTESIAN_POINT ( 'NONE',  ( -4.248408730893246776, -6.358192987158592047, -15.23635624981969627 ) ) ;
#1353 = CARTESIAN_POINT ( 'NONE',  ( 50.00000000000000000, 230.0000000000000000, -84.99999999999998579 ) ) ;
#1354 = VERTEX_POINT ( 'NONE', #2547 ) ;
#1355 = CARTESIAN_POINT ( 'NONE',  ( 4.941899431655324193, -20.93672964816920867, 76.30663123623098443 ) ) ;
#1356 = DIRECTION ( 'NONE',  ( -0.000000000000000000, -0.000000000000000000, 1.000000000000000000 ) ) ;
#1357 = DIRECTION ( 'NONE',  ( -1.000000000000000000, -0.000000000000000000, -0.000000000000000000 ) ) ;
#1358 = EDGE_CURVE ( 'NONE', #10315, #9271, #7170, .T. ) ;
#1359 = EDGE_CURVE ( 'NONE', #1568, #8829, #15366, .T. ) ;
#1360 = VECTOR ( 'NONE', #271, 1000.000000000000000 ) ;
#1361 = ORIENTED_EDGE ( 'NONE', *, *, #18493, .F. ) ;
#1362 = LINE ( 'NONE', #20629, #12090 ) ;
#1363 = LINE ( 'NONE', #9504, #8717 ) ;
#1364 = ORIENTED_EDGE ( 'NONE', *, *, #13741, .T. ) ;
#1365 = CARTESIAN_POINT ( 'NONE',  ( 0.000000000000000000, 46.17500197033058384, 55.24372537266413730 ) ) ;
#1366 = DIRECTION ( 'NONE',  ( -0.000000000000000000, -0.000000000000000000, 1.000000000000000000 ) ) ;
#1367 = CARTESIAN_POINT ( 'NONE',  ( -3.580422610670017658, 18.00000000043040771, -9.521831249819690868 ) ) ;
#1368 = EDGE_CURVE ( 'NONE', #14689, #5761, #15305, .T. ) ;
#1369 = VERTEX_POINT ( 'NONE', #15252 ) ;
#1370 = LINE ( 'NONE', #13867, #10372 ) ;
#1371 = DIRECTION ( 'NONE',  ( 0.000000000000000000, -0.8169698930104354329, -0.5766803221148765202 ) ) ;
#1372 = CARTESIAN_POINT ( 'NONE',  ( 0.000000000000000000, 0.000000000000000000, -68.00000000000000000 ) ) ;
#1373 = CARTESIAN_POINT ( 'NONE',  ( 42.61160110135224244, -124.0569253416645665, 88.80170281571383839 ) ) ;
#1374 = DIRECTION ( 'NONE',  ( -1.000000000000000000, -1.836909530733573776E-16, 0.000000000000000000 ) ) ;
#1375 = CARTESIAN_POINT ( 'NONE',  ( 3.580422614997669228, 17.99999999956958874, 11.82183125018031156 ) ) ;
#1376 = CARTESIAN_POINT ( 'NONE',  ( 7.500000000000007994, -9.015933403756345817E-10, -21.63629999981969121 ) ) ;
#1377 = VERTEX_POINT ( 'NONE', #13674 ) ;
#1378 = CARTESIAN_POINT ( 'NONE',  ( 0.000000000000000000, 0.000000000000000000, 0.000000000000000000 ) ) ;
#1379 = CARTESIAN_POINT ( 'NONE',  ( 8.382925368423265411, -12.54593441764187034, 11.59486433151907470 ) ) ;
#1380 = DIRECTION ( 'NONE',  ( -0.000000000000000000, -0.000000000000000000, 1.000000000000000000 ) ) ;
#1381 = AXIS2_PLACEMENT_3D ( 'NONE', #10449, #12141, #244 ) ;
#1382 = ORIENTED_EDGE ( 'NONE', *, *, #1219, .F. ) ;
#1383 = FACE_OUTER_BOUND ( 'NONE', #4278, .T. ) ;
#1384 = CARTESIAN_POINT ( 'NONE',  ( 2.163825119083639534E-09, 18.00000000000000000, -16.74769999981968738 ) ) ;
#1385 = CARTESIAN_POINT ( 'NONE',  ( 19.99999999999999645, 0.000000000000000000, 0.000000000000000000 ) ) ;
#1386 = ORIENTED_EDGE ( 'NONE', *, *, #9656, .F. ) ;
#1387 = CYLINDRICAL_SURFACE ( 'NONE', #406, 65.24900000006525147 ) ;
#1388 = ORIENTED_EDGE ( 'NONE', *, *, #9463, .T. ) ;
#1389 = CARTESIAN_POINT ( 'NONE',  ( 0.000000000000000000, -15.58726123847893774, 62.93731870009398932 ) ) ;
#1390 = CARTESIAN_POINT ( 'NONE',  ( 0.000000000000000000, -46.17500197033096754, 55.24372537266381755 ) ) ;
#1391 = CIRCLE ( 'NONE', #8796, 2.649999999999987477 ) ;
#1392 = ORIENTED_EDGE ( 'NONE', *, *, #18298, .T. ) ;
#1393 = ORIENTED_EDGE ( 'NONE', *, *, #12307, .F. ) ;
#1394 = CARTESIAN_POINT ( 'NONE',  ( 33.20850901831757795, -115.8985490652624435, -76.12077281629255765 ) ) ;
#1395 = AXIS2_PLACEMENT_3D ( 'NONE', #1849, #6710, #13290 ) ;
#1396 = DIRECTION ( 'NONE',  ( -0.000000000000000000, -0.000000000000000000, -1.000000000000000000 ) ) ;
#1397 = ADVANCED_FACE ( 'NONE', ( #17382 ), #12291, .T. ) ;
#1398 = EDGE_CURVE ( 'NONE', #10636, #1438, #1178, .T. ) ;
#1399 = LINE ( 'NONE', #15489, #20347 ) ;
#1400 = CARTESIAN_POINT ( 'NONE',  ( -6.330490856366295382, 9.474249098604511587, -15.02223399935257042 ) ) ;
#1401 = CARTESIAN_POINT ( 'NONE',  ( -5.303300858261583706, 5.303300859536630441, -22.01057499981969201 ) ) ;
#1402 = DIRECTION ( 'NONE',  ( 0.000000000000000000, -1.000000000000000000, 0.000000000000000000 ) ) ;
#1403 = FACE_OUTER_BOUND ( 'NONE', #10542, .T. ) ;
#1404 = CARTESIAN_POINT ( 'NONE',  ( 50.00000000000000000, 230.0000000000000000, 0.000000000000000000 ) ) ;
#1405 = ORIENTED_EDGE ( 'NONE', *, *, #20300, .T. ) ;
#1406 = DIRECTION ( 'NONE',  ( 1.000000000000000000, 0.000000000000000000, 0.000000000000000000 ) ) ;
#1407 = ORIENTED_EDGE ( 'NONE', *, *, #9613, .T. ) ;
#1408 = CARTESIAN_POINT ( 'NONE',  ( 2.163825119083639534E-09, 18.00000000000000000, -9.227299999819686960 ) ) ;
#1409 = CARTESIAN_POINT ( 'NONE',  ( 20.76542986210400699, -5.602711969362187183, 80.65560201174187682 ) ) ;
#1410 = CIRCLE ( 'NONE', #3427, 80.00000000000000000 ) ;
#1411 = VERTEX_POINT ( 'NONE', #7508 ) ;
#1412 = DIRECTION ( 'NONE',  ( -1.000000000000000000, -0.000000000000000000, 0.000000000000000000 ) ) ;
#1413 = ORIENTED_EDGE ( 'NONE', *, *, #9828, .T. ) ;
#1414 = FACE_BOUND ( 'NONE', #12896, .T. ) ;
#1415 = LINE ( 'NONE', #20481, #13457 ) ;
#1416 = LINE ( 'NONE', #7866, #7682 ) ;
#1417 = ORIENTED_EDGE ( 'NONE', *, *, #12888, .T. ) ;
#1418 = DIRECTION ( 'NONE',  ( -1.000000000000000000, 0.000000000000000000, 0.000000000000000000 ) ) ;
#1419 = CARTESIAN_POINT ( 'NONE',  ( -52.49999999999999289, -40.00000000000000000, 5.000000000000000000 ) ) ;
#1420 = CARTESIAN_POINT ( 'NONE',  ( 0.000000000000000000, -14.55863677812166124, 63.60407295269099137 ) ) ;
#1421 = CIRCLE ( 'NONE', #15324, 72.00000000007199219 ) ;
#1422 = CIRCLE ( 'NONE', #8837, 10.00000000000000178 ) ;
#1423 = ADVANCED_FACE ( 'NONE', ( #7302 ), #20234, .T. ) ;
#1424 = LINE ( 'NONE', #17631, #16707 ) ;
#1425 = VECTOR ( 'NONE', #15655, 1000.000000000000000 ) ;
#1426 = EDGE_LOOP ( 'NONE', ( #6656, #5108, #124, #16239 ) ) ;
#1427 = DIRECTION ( 'NONE',  ( -0.000000000000000000, -0.000000000000000000, -1.000000000000000000 ) ) ;
#1428 = DIRECTION ( 'NONE',  ( -1.000000000000000000, 0.000000000000000000, 0.000000000000000000 ) ) ;
#1429 = VERTEX_POINT ( 'NONE', #17174 ) ;
#1430 = CARTESIAN_POINT ( 'NONE',  ( -6.165580000000000283, 1.321856812770071588E-15, -10.79377999999999993 ) ) ;
#1431 = DIRECTION ( 'NONE',  ( 0.000000000000000000, 0.000000000000000000, -1.000000000000000000 ) ) ;
#1432 = ADVANCED_FACE ( 'NONE', ( #2657 ), #15568, .T. ) ;
#1433 = VERTEX_POINT ( 'NONE', #12401 ) ;
#1434 = DIRECTION ( 'NONE',  ( -1.000000000000000000, -0.000000000000000000, -0.000000000000000000 ) ) ;
#1435 = CARTESIAN_POINT ( 'NONE',  ( 50.00000000000000000, -159.9999999999999716, -85.00000000000000000 ) ) ;
#1436 = CARTESIAN_POINT ( 'NONE',  ( 6.250000000000054179, 10.82531754730546147, 166.0000000000000000 ) ) ;
#1437 = VECTOR ( 'NONE', #5990, 1000.000000000000000 ) ;
#1438 = VERTEX_POINT ( 'NONE', #18872 ) ;
#1439 = AXIS2_PLACEMENT_3D ( 'NONE', #1624, #11245, #8269 ) ;
#1440 = DIRECTION ( 'NONE',  ( 0.000000000000000000, 0.7308359642781206977, 0.6825531432186578984 ) ) ;
#1441 = ORIENTED_EDGE ( 'NONE', *, *, #9365, .F. ) ;
#1442 = DIRECTION ( 'NONE',  ( -1.000000000000000000, 0.000000000000000000, 0.000000000000000000 ) ) ;
#1443 = CIRCLE ( 'NONE', #1108, 8.500000000000000000 ) ;
#1444 = EDGE_CURVE ( 'NONE', #14263, #20655, #16203, .T. ) ;
#1445 = ORIENTED_EDGE ( 'NONE', *, *, #14802, .T. ) ;
#1446 = EDGE_CURVE ( 'NONE', #2775, #12799, #7943, .T. ) ;
#1447 = CARTESIAN_POINT ( 'NONE',  ( 19.99999999999999645, -24.01204443665229604, 60.22865198596116443 ) ) ;
#1448 = DIRECTION ( 'NONE',  ( -1.000000000000000000, -0.000000000000000000, 0.000000000000000000 ) ) ;
#1449 = ITEM_DEFINED_TRANSFORMATION ( 'NONE', 'NONE', #18452,  #12461 ) ;
#1450 = CARTESIAN_POINT ( 'NONE',  ( -1.343452921478824119E-09, -11.17563879731705789, 18.84885975064742425 ) ) ;
#1451 = VECTOR ( 'NONE', #2646, 1000.000000000000000 ) ;
#1453 = ORIENTED_EDGE ( 'NONE', *, *, #19628, .T. ) ;
#1452 = AXIS2_PLACEMENT_3D ( 'NONE', #4891, #4778, #12644 ) ;
#1454 = CARTESIAN_POINT ( 'NONE',  ( 2.870125741905212635, -6.929096494179677101, -16.70901249981969272 ) ) ;
#1455 = FACE_BOUND ( 'NONE', #20340, .T. ) ;
#1456 = AXIS2_PLACEMENT_3D ( 'NONE', #495, #8223, #10027 ) ;
#1457 = ORIENTED_EDGE ( 'NONE', *, *, #16113, .F. ) ;
#1458 = ADVANCED_FACE ( 'NONE', ( #8139 ), #20860, .T. ) ;
#1459 = EDGE_CURVE ( 'NONE', #8383, #8626, #18037, .T. ) ;
#1460 = CARTESIAN_POINT ( 'NONE',  ( -6.929096493489627306, 2.870125743571138699, -22.59963749981969627 ) ) ;
#1461 = FACE_OUTER_BOUND ( 'NONE', #9867, .T. ) ;
#1462 = TOROIDAL_SURFACE ( 'NONE', #430, 10.79377999999999993, 0.06721999999999977993 ) ;
#1463 = EDGE_LOOP ( 'NONE', ( #3145, #5922, #2992, #2618 ) ) ;
#1464 = ADVANCED_FACE ( 'NONE', ( #14613 ), #19375, .T. ) ;
#1465 = CARTESIAN_POINT ( 'NONE',  ( 0.000000000000000000, 0.000000000000000000, 46.00000000000000711 ) ) ;
#1466 = LINE ( 'NONE', #9410, #16845 ) ;
#1467 = ADVANCED_FACE ( 'NONE', ( #12829 ), #6545, .T. ) ;
#1468 = VERTEX_POINT ( 'NONE', #9321 ) ;
#1469 = AXIS2_PLACEMENT_3D ( 'NONE', #18399, #13530, #5455 ) ;
#1470 = CARTESIAN_POINT ( 'NONE',  ( -19.56341920831713210, -12.11112665530244925, -81.72775504840210203 ) ) ;
#1471 = CIRCLE ( 'NONE', #19391, 8.999999999999998224 ) ;
#1472 = CARTESIAN_POINT ( 'NONE',  ( 11.50000000000000000, 0.000000000000000000, 68.00000000000000000 ) ) ;
#1473 = MECHANICAL_DESIGN_GEOMETRIC_PRESENTATION_REPRESENTATION (  '', ( #5158 ), #7492 ) ;
#1474 = CARTESIAN_POINT ( 'NONE',  ( -9.850000000000012079, 3.245314017740477087E-16, 129.0000000000000000 ) ) ;
#1475 = COLOUR_RGB ( '', 0.09019608, 0.27058824, 0.51372549) ;
#1476 = ORIENTED_EDGE ( 'NONE', *, *, #20774, .F. ) ;
#1477 = CARTESIAN_POINT ( 'NONE',  ( -7.500000000000000000, 0.000000000000000000, 40.00000000000000000 ) ) ;
#1478 = FILL_AREA_STYLE ('',( #6332 ) ) ;
#1479 = DIRECTION ( 'NONE',  ( -0.000000000000000000, -0.000000000000000000, 1.000000000000000000 ) ) ;
#1480 = DIRECTION ( 'NONE',  ( 0.000000000000000000, 0.000000000000000000, 1.000000000000000000 ) ) ;
#1481 = EDGE_CURVE ( 'NONE', #18587, #17728, #20405, .T. ) ;
#1482 = CIRCLE ( 'NONE', #13313, 20.00000000000000000 ) ;
#1483 = CARTESIAN_POINT ( 'NONE',  ( -10.19618095047498230, 15.25966317163203279, -17.63129374981969377 ) ) ;
#1484 = EDGE_CURVE ( 'NONE', #18498, #3220, #443, .T. ) ;
#1485 = CARTESIAN_POINT ( 'NONE',  ( 7.499999999820668783, -1.491842756249033508, -11.91676874981968659 ) ) ;
#1486 = CIRCLE ( 'NONE', #5867, 2.700000000000000622 ) ;
#1487 = FACE_BOUND ( 'NONE', #13030, .T. ) ;
#1488 = AXIS2_PLACEMENT_3D ( 'NONE', #350, #19238, #4715 ) ;
#1489 = CARTESIAN_POINT ( 'NONE',  ( 10.46442989202483531, -10.46442989454075168, -7.549666918480926192 ) ) ;
#1490 = EDGE_CURVE ( 'NONE', #9017, #17731, #20650, .T. ) ;
#1491 = LINE ( 'NONE', #4549, #19305 ) ;
#1492 = VERTEX_POINT ( 'NONE', #17905 ) ;
#1493 = DIRECTION ( 'NONE',  ( 0.000000000000000000, 0.000000000000000000, 1.000000000000000000 ) ) ;
#1494 = DIRECTION ( 'NONE',  ( -0.4999999999999918954, 0.8660254037844433705, 0.000000000000000000 ) ) ;
#1495 = DIRECTION ( 'NONE',  ( 1.734723475976806848E-16, 1.000000000000000000, 0.000000000000000000 ) ) ;
#1496 = CIRCLE ( 'NONE', #468, 2.650000000000000355 ) ;
#1497 = ORIENTED_EDGE ( 'NONE', *, *, #14164, .F. ) ;
#1498 = CONICAL_SURFACE ( 'NONE', #4183, 2.055000000000000160, 0.7853981633974633780 ) ;
#1499 = CARTESIAN_POINT ( 'NONE',  ( 2.500000000000000000, 2.357898499370431722, -2.818925648462311528E-15 ) ) ;
#1500 = ORIENTED_EDGE ( 'NONE', *, *, #19442, .T. ) ;
#1501 = CARTESIAN_POINT ( 'NONE',  ( 50.00000000000000000, 31.35083268962916137, 50.63110039191614220 ) ) ;
#1502 = CARTESIAN_POINT ( 'NONE',  ( -17.99999999956958163, 3.580422614997673669, 16.98598125018031268 ) ) ;
#1503 = ORIENTED_EDGE ( 'NONE', *, *, #2780, .T. ) ;
#1504 = ORIENTED_EDGE ( 'NONE', *, *, #13362, .F. ) ;
#1505 = DIRECTION ( 'NONE',  ( -1.000000000000000000, 0.000000000000000000, 0.000000000000000000 ) ) ;
#1506 = VECTOR ( 'NONE', #14655, 1000.000000000000000 ) ;
#1507 = CIRCLE ( 'NONE', #3494, 27.60000000002759535 ) ;
#1508 = FILL_AREA_STYLE_COLOUR ( '', #14117 ) ;
#1509 = CARTESIAN_POINT ( 'NONE',  ( 19.99999999999999645, -42.42902769288503606, -49.02903636734241388 ) ) ;
#1510 = EDGE_CURVE ( 'NONE', #880, #7974, #1471, .T. ) ;
#1511 = LINE ( 'NONE', #14435, #17019 ) ;
#1512 = CARTESIAN_POINT ( 'NONE',  ( -4.276731812588566939, 10.32494394809439875, -5.302702749352572020 ) ) ;
#1513 = CARTESIAN_POINT ( 'NONE',  ( -6.358192988180014993, -4.248408729364575365, -24.07229374981969627 ) ) ;
#1514 = CARTESIAN_POINT ( 'NONE',  ( 8.899999999999895550, -10.82531754730554496, 126.0000000000000000 ) ) ;
#1515 = CARTESIAN_POINT ( 'NONE',  ( 0.000000000000000000, 0.000000000000000000, 0.000000000000000000 ) ) ;
#1516 = DIRECTION ( 'NONE',  ( -0.4999999999999918954, 0.8660254037844433705, 0.000000000000000000 ) ) ;
#1517 = AXIS2_PLACEMENT_3D ( 'NONE', #7998, #14477, #2807 ) ;
#1518 = VERTEX_POINT ( 'NONE', #17804 ) ;
#1519 = CARTESIAN_POINT ( 'NONE',  ( 19.99999999999999645, 15.58726123847937828, -62.93731870009387563 ) ) ;
#1520 = ORIENTED_EDGE ( 'NONE', *, *, #10012, .F. ) ;
#1521 = CARTESIAN_POINT ( 'NONE',  ( 10.19618095414378800, 15.25966316918061416, -17.76870624981969016 ) ) ;
#1522 = CARTESIAN_POINT ( 'NONE',  ( 50.00000000000000000, 31.35083268962916137, -50.63110039191615641 ) ) ;
#1523 = ORIENTED_EDGE ( 'NONE', *, *, #14301, .F. ) ;
#1524 = CARTESIAN_POINT ( 'NONE',  ( 0.000000000000000000, 0.000000000000000000, 0.000000000000000000 ) ) ;
#1525 = ORIENTED_EDGE ( 'NONE', *, *, #2233, .F. ) ;
#1526 = LINE ( 'NONE', #20792, #14248 ) ;
#1527 = DIRECTION ( 'NONE',  ( -1.000000000000000000, 0.000000000000000000, 0.000000000000000000 ) ) ;
#1528 = CARTESIAN_POINT ( 'NONE',  ( -6.929096493489627306, 2.870125743571138699, -3.749637499819692632 ) ) ;
#1529 = EDGE_CURVE ( 'NONE', #14269, #13959, #7882, .T. ) ;
#1530 = AXIS2_PLACEMENT_3D ( 'NONE', #13066, #19523, #12966 ) ;
#1531 = ORIENTED_EDGE ( 'NONE', *, *, #2872, .F. ) ;
#1532 = FACE_OUTER_BOUND ( 'NONE', #6468, .T. ) ;
#1533 = FACE_OUTER_BOUND ( 'NONE', #4714, .T. ) ;
#1534 = CYLINDRICAL_SURFACE ( 'NONE', #20447, 4.250000000000000000 ) ;
#1535 = DIRECTION ( 'NONE',  ( 0.000000000000000000, -0.8660254037844390407, -0.4999999999999994449 ) ) ;
#1536 = VERTEX_POINT ( 'NONE', #9739 ) ;
#1537 = CARTESIAN_POINT ( 'NONE',  ( -15.15000000000000036, 3.245314017740478073E-16, 46.00000000000000711 ) ) ;
#1538 = CARTESIAN_POINT ( 'NONE',  ( 0.000000000000000000, -55.05624179292004072, 35.01774179823764399 ) ) ;
#1539 = VERTEX_POINT ( 'NONE', #14206 ) ;
#1540 = COLOUR_RGB ( '', 0.31764706, 0.68627451, 0.89019608) ;
#1541 = CARTESIAN_POINT ( 'NONE',  ( 0.000000000000000000, 64.79224928664392280, -2.456263514197840614 ) ) ;
#1542 = DIRECTION ( 'NONE',  ( -1.000000000000000000, -0.000000000000000000, -0.000000000000000000 ) ) ;
#1543 = ORIENTED_EDGE ( 'NONE', *, *, #11308, .F. ) ;
#1544 = LINE ( 'NONE', #17949, #7850 ) ;
#1545 = FACE_OUTER_BOUND ( 'NONE', #6841, .T. ) ;
#1546 = CYLINDRICAL_SURFACE ( 'NONE', #492, 11.50000000000000000 ) ;
#1547 = EDGE_LOOP ( 'NONE', ( #5502, #13967, #18931, #4600 ) ) ;
#1548 = CARTESIAN_POINT ( 'NONE',  ( 62.49999999999999289, -30.00000000000000000, 5.000000000000000000 ) ) ;
#1549 = ORIENTED_EDGE ( 'NONE', *, *, #18148, .T. ) ;
#1550 = AXIS2_PLACEMENT_3D ( 'NONE', #2111, #8569, #15046 ) ;
#1551 = DIRECTION ( 'NONE',  ( 1.000000000000000000, 0.000000000000000000, 0.000000000000000000 ) ) ;
#1552 = ADVANCED_FACE ( 'NONE', ( #6132 ), #11012, .T. ) ;
#1553 = VERTEX_POINT ( 'NONE', #6240 ) ;
#1554 = CARTESIAN_POINT ( 'NONE',  ( 36.52125820097372610, -119.8000680387651187, 78.43373391519315874 ) ) ;
#1555 = EDGE_CURVE ( 'NONE', #6474, #18397, #14521, .T. ) ;
#1556 = DIRECTION ( 'NONE',  ( -1.000000000000000000, 0.000000000000000000, 0.000000000000000000 ) ) ;
#1557 = CARTESIAN_POINT ( 'NONE',  ( -12.54593441562641054, 8.382925371439629458, -16.36361433115845898 ) ) ;
#1558 = EDGE_LOOP ( 'NONE', ( #5571, #10917, #2045 ) ) ;
#1559 = CIRCLE ( 'NONE', #12741, 27.60000000002760245 ) ;
#1560 = DIRECTION ( 'NONE',  ( -8.673617379884035472E-17, 1.000000000000000000, 0.000000000000000000 ) ) ;
#1561 = DIRECTION ( 'NONE',  ( -1.000000000000000000, -0.000000000000000000, -0.000000000000000000 ) ) ;
#1562 = EDGE_LOOP ( 'NONE', ( #2821, #6138, #7400, #885, #13620 ) ) ;
#1563 =( BOUNDED_CURVE ( )  B_SPLINE_CURVE ( 2, ( #10433, #16893, #2370, #8822, #9368, #5969, #19123, #7771, #16041, #12341, #6283, #17539, #9568, #17217, #11063, #14149, #12446 ),
 .UNSPECIFIED., .F., .T. ) 
 B_SPLINE_CURVE_WITH_KNOTS ( ( 3, 2, 2, 2, 2, 2, 2, 2, 3 ),
 ( 0.1000000000038511888, 0.1125000000038511860, 0.1250000000038511694, 0.1375000000038511805, 0.1500000000038511638, 0.1625000000038511749, 0.1750000000038511583, 0.1875000000038511694, 0.2000000000038511805 ),
 .UNSPECIFIED. ) 
 CURVE ( )  GEOMETRIC_REPRESENTATION_ITEM ( )  RATIONAL_B_SPLINE_CURVE ( ( 0.9999999999940800688, 0.9807852804091503618, 1.000000000000000000, 0.9807852804032304306, 1.000000000000000000, 0.9807852804032304306, 1.000000000000000000, 0.9807852804032304306, 1.000000000000000000, 0.9807852804032304306, 1.000000000000000000, 0.9807852804032304306, 1.000000000000000000, 0.9807852804032304306, 1.000000000000000000, 0.9807852803973104994, 1.000000000005919931 ) ) 
 REPRESENTATION_ITEM ( '' )  );
#1564 = CARTESIAN_POINT ( 'NONE',  ( 15.98236128136674949, -14.38466504862504358, 80.08563004779874461 ) ) ;
#1565 = CARTESIAN_POINT ( 'NONE',  ( 15.25966317163202746, 10.19618095047498407, 22.42495625018031191 ) ) ;
#1566 = DIRECTION ( 'NONE',  ( 0.000000000000000000, 0.000000000000000000, -1.000000000000000000 ) ) ;
#1567 = DIRECTION ( 'NONE',  ( 0.000000000000000000, -0.000000000000000000, 1.000000000000000000 ) ) ;
#1568 = VERTEX_POINT ( 'NONE', #17489 ) ;
#1569 = FACE_BOUND ( 'NONE', #6597, .T. ) ;
#1570 = DIRECTION ( 'NONE',  ( -1.000000000000000000, 0.000000000000000000, -0.000000000000000000 ) ) ;
#1571 = VERTEX_POINT ( 'NONE', #2966 ) ;
#1572 = FACE_OUTER_BOUND ( 'NONE', #15707, .T. ) ;
#1573 = AXIS2_PLACEMENT_3D ( 'NONE', #14225, #20577, #1198 ) ;
#1574 = FACE_OUTER_BOUND ( 'NONE', #17556, .T. ) ;
#1575 = CARTESIAN_POINT ( 'NONE',  ( 5.000000000000002665, 3.306546357697854226E-16, 2.700000000000000622 ) ) ;
#1576 = ORIENTED_EDGE ( 'NONE', *, *, #7144, .F. ) ;
#1577 = CARTESIAN_POINT ( 'NONE',  ( 50.00000000000000000, -160.0000000000000000, 0.000000000000000000 ) ) ;
#1578 = ADVANCED_FACE ( 'NONE', ( #9431, #1383 ), #14312, .T. ) ;
#1579 = FILL_AREA_STYLE ('',( #14294 ) ) ;
#1580 = EDGE_CURVE ( 'NONE', #3802, #19413, #19723, .T. ) ;
#1581 = CYLINDRICAL_SURFACE ( 'NONE', #105, 10.52399999999999380 ) ;
#1582 = DIRECTION ( 'NONE',  ( -9.719167153370763981E-31, -1.472034489194787016E-30, -1.000000000000000000 ) ) ;
#1583 = CARTESIAN_POINT ( 'NONE',  ( 16.62983158437509701, -6.888301784570740161, -13.80238749981969271 ) ) ;
#1584 = EDGE_LOOP ( 'NONE', ( #432, #16666 ) ) ;
#1585 = VECTOR ( 'NONE', #7418, 1000.000000000000000 ) ;
#1586 = CARTESIAN_POINT ( 'NONE',  ( 0.000000000000000000, 64.79224928664392280, -2.456263514197840614 ) ) ;
#1587 = EDGE_CURVE ( 'NONE', #17270, #8626, #15654, .T. ) ;
#1588 = CARTESIAN_POINT ( 'NONE',  ( -6.679999999999998828, 4.605132193549069780E-15, 0.000000000000000000 ) ) ;
#1589 = AXIS2_PLACEMENT_3D ( 'NONE', #13396, #14977, #3419 ) ;
#1590 = CONICAL_SURFACE ( 'NONE', #1904, 2.500000000000002220, 0.9599310885968777018 ) ;
#1591 = CARTESIAN_POINT ( 'NONE',  ( -1.779019326032424095E-09, -14.79893867758296544, 3.053458081519074163 ) ) ;
#1592 = CARTESIAN_POINT ( 'NONE',  ( -31.75000000000000000, 0.000000000000000000, 0.000000000000000000 ) ) ;
#1593 = ORIENTED_EDGE ( 'NONE', *, *, #12629, .T. ) ;
#1594 = CARTESIAN_POINT ( 'NONE',  ( 150.0000507999999968, 5.400000000000000355, -1.000000000000000000 ) ) ;
#1595 = AXIS2_PLACEMENT_3D ( 'NONE', #3914, #8901, #10179 ) ;
#1596 = CARTESIAN_POINT ( 'NONE',  ( -2.870125741905213079, 6.929096494179683319, 22.54338750018031590 ) ) ;
#1597 = FACE_OUTER_BOUND ( 'NONE', #513, .T. ) ;
#1598 = VERTEX_POINT ( 'NONE', #16907 ) ;
#1599 = ADVANCED_FACE ( 'NONE', ( #13730, #12239 ), #7248, .T. ) ;
#1600 = CARTESIAN_POINT ( 'NONE',  ( 0.000000000000000000, 0.000000000000000000, 0.000000000000000000 ) ) ;
#1601 = AXIS2_PLACEMENT_3D ( 'NONE', #888, #7553, #4483 ) ;
#1602 = EDGE_LOOP ( 'NONE', ( #19739, #6514, #5985, #17463 ) ) ;
#1603 = DIRECTION ( 'NONE',  ( 0.000000000000000000, -0.3984010898462485573, 0.9172113015054500496 ) ) ;
#1604 = CARTESIAN_POINT ( 'NONE',  ( 0.000000000000000000, 0.000000000000000000, 68.00000000000000000 ) ) ;
#1605 = CIRCLE ( 'NONE', #20184, 40.00000000000000000 ) ;
#1606 = ORIENTED_EDGE ( 'NONE', *, *, #4835, .F. ) ;
#1607 = VERTEX_POINT ( 'NONE', #11521 ) ;
#1608 = DIRECTION ( 'NONE',  ( -1.000000000000000000, 0.000000000000000000, -0.000000000000000000 ) ) ;
#1609 = EDGE_CURVE ( 'NONE', #9297, #4671, #18361, .T. ) ;
#1610 = STYLED_ITEM ( 'NONE', ( #17077 ), #19794 ) ;
#1611 = EDGE_CURVE ( 'NONE', #8077, #16773, #5553, .T. ) ;
#1612 =( NAMED_UNIT ( * ) PLANE_ANGLE_UNIT ( ) SI_UNIT ( $, .RADIAN. ) );
#1613 = DIRECTION ( 'NONE',  ( 0.000000000000000000, 0.000000000000000000, -1.000000000000000000 ) ) ;
#1614 = EDGE_CURVE ( 'NONE', #20241, #9722, #13622, .T. ) ;
#1615 = CARTESIAN_POINT ( 'NONE',  ( -6.929096493489632635, 2.870125743571140919, 11.94026250018031554 ) ) ;
#1616 = CARTESIAN_POINT ( 'NONE',  ( 10.32494394706615637, -4.276731815070946574, 0.5339527497131985045 ) ) ;
#1617 = AXIS2_PLACEMENT_3D ( 'NONE', #8638, #6834, #18196 ) ;
#1618 = CARTESIAN_POINT ( 'NONE',  ( -6.177131623262581250, 0.000000000000000000, 0.000000000000000000 ) ) ;
#1619 = DIRECTION ( 'NONE',  ( -1.000000000000000000, -0.000000000000000000, -0.000000000000000000 ) ) ;
#1620 = CARTESIAN_POINT ( 'NONE',  ( -31.75000000000000000, 10.85999999999999410, 0.000000000000000000 ) ) ;
#1621 = AXIS2_PLACEMENT_3D ( 'NONE', #10484, #20229, #7617 ) ;
#1622 = EDGE_LOOP ( 'NONE', ( #15502, #16307, #20064, #1757 ) ) ;
#1623 = VECTOR ( 'NONE', #9712, 1000.000000000000000 ) ;
#1624 = CARTESIAN_POINT ( 'NONE',  ( 0.000000000000000000, 0.000000000000000000, 0.000000000000000000 ) ) ;
#1625 = VERTEX_POINT ( 'NONE', #11630 ) ;
#1626 = CARTESIAN_POINT ( 'NONE',  ( 18.00000000043041126, 3.580422610670019434, 23.01401875018031262 ) ) ;
#1627 = CARTESIAN_POINT ( 'NONE',  ( 0.000000000000000000, 3.141410481201988070, -65.17333458706183080 ) ) ;
#1628 = VERTEX_POINT ( 'NONE', #3966 ) ;
#1629 = EDGE_CURVE ( 'NONE', #9402, #16949, #2802, .T. ) ;
#1630 = DIRECTION ( 'NONE',  ( 0.000000000000000000, 0.000000000000000000, -1.000000000000000000 ) ) ;
#1631 = VERTEX_POINT ( 'NONE', #1787 ) ;
#1632 = EDGE_CURVE ( 'NONE', #3634, #12603, #12137, .T. ) ;
#1633 = FACE_OUTER_BOUND ( 'NONE', #20105, .T. ) ;
#1634 = CARTESIAN_POINT ( 'NONE',  ( 2.681483223904247648, -3.070647092368467224, -5.599999999999980105 ) ) ;
#1635 = ORIENTED_EDGE ( 'NONE', *, *, #6502, .T. ) ;
#1636 = CIRCLE ( 'NONE', #9062, 27.60000000002759890 ) ;
#1637 = ORIENTED_EDGE ( 'NONE', *, *, #18433, .F. ) ;
#1638 = DIRECTION ( 'NONE',  ( 1.000000000000000000, -0.000000000000000000, -0.000000000000000000 ) ) ;
#1639 = CIRCLE ( 'NONE', #10071, 14.49999999999999467 ) ;
#1640 = ADVANCED_FACE ( 'NONE', ( #6651 ), #8838, .T. ) ;
#1641 = CARTESIAN_POINT ( 'NONE',  ( 0.000000000000000000, -46.01927912072559224, 45.67597560296373871 ) ) ;
#1642 = STYLED_ITEM ( 'NONE', ( #16647 ), #7446 ) ;
#1643 = DIRECTION ( 'NONE',  ( -0.000000000000000000, -0.000000000000000000, 1.000000000000000000 ) ) ;
#1644 = VERTEX_POINT ( 'NONE', #15313 ) ;
#1645 = CARTESIAN_POINT ( 'NONE',  ( 9.015937996181834148E-10, 7.500000000000000888, 7.442550000180311542 ) ) ;
#1646 = EDGE_CURVE ( 'NONE', #3206, #4597, #5057, .T. ) ;
#1647 = CARTESIAN_POINT ( 'NONE',  ( 9.000000000000007105, -85.00000000000000000, 5.000000000000000000 ) ) ;
#1648 = LINE ( 'NONE', #13177, #18750 ) ;
#1649 = LINE ( 'NONE', #1737, #19416 ) ;
#1650 = ORIENTED_EDGE ( 'NONE', *, *, #1510, .F. ) ;
#1651 = LINE ( 'NONE', #3327, #12576 ) ;
#1652 = CARTESIAN_POINT ( 'NONE',  ( -3.580422610670018546, 18.00000000043041126, 18.75316875018031482 ) ) ;
#1653 = DIRECTION ( 'NONE',  ( 0.000000000000000000, -0.8878852184023795502, 0.4600650377311439332 ) ) ;
#1654 = ORIENTED_EDGE ( 'NONE', *, *, #18193, .T. ) ;
#1655 = FACE_BOUND ( 'NONE', #7489, .T. ) ;
#1656 = VERTEX_POINT ( 'NONE', #2285 ) ;
#1657 = DIRECTION ( 'NONE',  ( -1.000000000000000000, -0.000000000000000000, -0.000000000000000000 ) ) ;
#1658 = ORIENTED_EDGE ( 'NONE', *, *, #7260, .T. ) ;
#1659 = CARTESIAN_POINT ( 'NONE',  ( 35.31732902261087048, -118.6065303221148071, 77.66260182251970434 ) ) ;
#1660 = DIRECTION ( 'NONE',  ( 0.000000000000000000, 0.000000000000000000, -1.000000000000000000 ) ) ;
#1661 = CARTESIAN_POINT ( 'NONE',  ( -5.663308650141539502, -13.67243654642775574, -19.01439558115845685 ) ) ;
#1662 = ADVANCED_FACE ( 'NONE', ( #13136 ), #10549, .T. ) ;
#1663 = ORIENTED_EDGE ( 'NONE', *, *, #3369, .F. ) ;
#1664 = CARTESIAN_POINT ( 'NONE',  ( 50.00000000000000000, -164.9999999999999716, 50.00000000000001421 ) ) ;
#1665 = EDGE_CURVE ( 'NONE', #13788, #3825, #18718, .T. ) ;
#1666 = DIRECTION ( 'NONE',  ( 0.000000000000000000, 0.000000000000000000, 1.000000000000000000 ) ) ;
#1667 = EDGE_LOOP ( 'NONE', ( #13083, #11527, #16791, #852 ) ) ;
#1668 = CARTESIAN_POINT ( 'NONE',  ( 6.929096493489625530, -2.870125743571142252, -27.31213749981969485 ) ) ;
#1669 = CARTESIAN_POINT ( 'NONE',  ( -17.99999999956958519, 3.580422614997674113, 18.89058125018031475 ) ) ;
#1670 = LINE ( 'NONE', #9006, #11754 ) ;
#1671 = DIRECTION ( 'NONE',  ( 0.000000000000000000, 0.000000000000000000, 1.000000000000000000 ) ) ;
#1672 = EDGE_LOOP ( 'NONE', ( #10230, #4922, #16912, #8374 ) ) ;
#1673 = DIRECTION ( 'NONE',  ( 0.000000000000000000, 0.000000000000000000, 1.000000000000000000 ) ) ;
#1674 = ORIENTED_EDGE ( 'NONE', *, *, #8973, .F. ) ;
#1675 = CARTESIAN_POINT ( 'NONE',  ( -12.23225220234714072, -19.49129496293704733, -77.02726945203133369 ) ) ;
#1676 = DIRECTION ( 'NONE',  ( 0.000000000000000000, 0.3984010898462422290, -0.9172113015054527141 ) ) ;
#1677 = CARTESIAN_POINT ( 'NONE',  ( 4.248408730893249441, 6.358192987158596488, -4.258956249819687123 ) ) ;
#1678 = ORIENTED_EDGE ( 'NONE', *, *, #17127, .F. ) ;
#1679 = ADVANCED_FACE ( 'NONE', ( #20071 ), #8955, .T. ) ;
#1680 = DIRECTION ( 'NONE',  ( -1.000000000000000000, 0.000000000000000000, 0.000000000000000000 ) ) ;
#1681 = LINE ( 'NONE', #17450, #12263 ) ;
#1682 =( NAMED_UNIT ( * ) SI_UNIT ( $, .STERADIAN. ) SOLID_ANGLE_UNIT ( ) );
#1683 = CARTESIAN_POINT ( 'NONE',  ( -18.00000000000000355, 2.163826221265759298E-09, -9.678949999819691286 ) ) ;
#1684 = VERTEX_POINT ( 'NONE', #15421 ) ;
#1685 = CARTESIAN_POINT ( 'NONE',  ( -17.50000000000000355, 0.000000000000000000, -43.00000000000000000 ) ) ;
#1686 = FACE_OUTER_BOUND ( 'NONE', #14854, .T. ) ;
#1687 = CARTESIAN_POINT ( 'NONE',  ( 8.382925371439627682, 12.54593441562639988, -0.7754481684809252373 ) ) ;
#1688 = DIRECTION ( 'NONE',  ( 0.000000000000000000, 0.000000000000000000, -1.000000000000000000 ) ) ;
#1689 = B_SPLINE_CURVE_WITH_KNOTS ( 'NONE', 3,
 ( #379, #3866, #2076, #8848, #6943, #13431 ),
 .UNSPECIFIED., .F., .F.,
 ( 4, 2, 4 ),
 ( 0.002336974151641576809, 0.003500975885716453226, 0.004664977619791330077 ),
 .UNSPECIFIED. ) ;
#1690 = EDGE_CURVE ( 'NONE', #19413, #3802, #9231, .T. ) ;
#1691 = ORIENTED_EDGE ( 'NONE', *, *, #6877, .F. ) ;
#1692 = CARTESIAN_POINT ( 'NONE',  ( 0.000000000000000000, 0.000000000000000000, 0.000000000000000000 ) ) ;
#1693 = DIRECTION ( 'NONE',  ( -1.000000000000000000, 0.000000000000000000, -0.000000000000000000 ) ) ;
#1694 = CARTESIAN_POINT ( 'NONE',  ( 30.18435758154164006, -45.05736527963534144, 66.43021625834032307 ) ) ;
#1695 = ORIENTED_EDGE ( 'NONE', *, *, #1690, .F. ) ;
#1696 = CARTESIAN_POINT ( 'NONE',  ( 0.000000000000000000, -71.89099403602352822, -3.960426305689553228 ) ) ;
#1697 = ORIENTED_EDGE ( 'NONE', *, *, #10399, .T. ) ;
#1698 = DIRECTION ( 'NONE',  ( -0.000000000000000000, -0.000000000000000000, 1.000000000000000000 ) ) ;
#1699 = ORIENTED_EDGE ( 'NONE', *, *, #11165, .T. ) ;
#1700 = ORIENTED_EDGE ( 'NONE', *, *, #1882, .T. ) ;
#1701 = DIRECTION ( 'NONE',  ( -1.000000000000000000, 0.000000000000000000, 0.000000000000000000 ) ) ;
#1702 = EDGE_CURVE ( 'NONE', #1069, #14401, #6749, .T. ) ;
#1703 = CIRCLE ( 'NONE', #8439, 54.99999999999999289 ) ;
#1704 = CARTESIAN_POINT ( 'NONE',  ( 19.99999999999999645, 36.54710069451054011, 54.05313526368126276 ) ) ;
#1705 = DIRECTION ( 'NONE',  ( 0.000000000000000000, 1.000000000000000000, 0.000000000000000000 ) ) ;
#1706 = CYLINDRICAL_SURFACE ( 'NONE', #19725, 72.00000000007199219 ) ;
#1707 = CARTESIAN_POINT ( 'NONE',  ( -7.499999999820669672, 1.491842756249032620, 21.07073125018031945 ) ) ;
#1708 = CARTESIAN_POINT ( 'NONE',  ( 1.343451552857795099E-09, 11.17563879731704723, -2.411359750286803827 ) ) ;
#1709 = FACE_BOUND ( 'NONE', #7019, .T. ) ;
#1710 = CARTESIAN_POINT ( 'NONE',  ( 0.000000000000000000, 0.000000000000000000, 68.00000000000000000 ) ) ;
#1711 = EDGE_CURVE ( 'NONE', #1631, #18530, #909, .T. ) ;
#1712 = EDGE_LOOP ( 'NONE', ( #16835, #8897, #8810, #11295 ) ) ;
#1713 = CYLINDRICAL_SURFACE ( 'NONE', #1452, 27.60000000002759535 ) ;
#1714 = EDGE_CURVE ( 'NONE', #12603, #20554, #11925, .T. ) ;
#1715 = CARTESIAN_POINT ( 'NONE',  ( -10.19618095414378622, -15.25966316918061416, 7.698393750180313688 ) ) ;
#1716 = DIRECTION ( 'NONE',  ( 1.000000000000000000, -0.000000000000000000, -0.000000000000000000 ) ) ;
#1717 = VERTEX_POINT ( 'NONE', #20608 ) ;
#1718 = DIRECTION ( 'NONE',  ( 1.000000000000000000, 0.000000000000000000, 0.000000000000000000 ) ) ;
#1719 = EDGE_LOOP ( 'NONE', ( #16206, #15412 ) ) ;
#1720 = CARTESIAN_POINT ( 'NONE',  ( 9.999999999999998224, 59.36728637278019960, 40.73727173906807764 ) ) ;
#1721 = CARTESIAN_POINT ( 'NONE',  ( 30.43430782549248903, -42.57363661491096707, -66.38288848018790134 ) ) ;
#1722 = EDGE_CURVE ( 'NONE', #18079, #19080, #12964, .T. ) ;
#1723 = ORIENTED_EDGE ( 'NONE', *, *, #16442, .T. ) ;
#1724 = VECTOR ( 'NONE', #19074, 1000.000000000000000 ) ;
#1725 = ORIENTED_EDGE ( 'NONE', *, *, #10894, .T. ) ;
#1726 = DIRECTION ( 'NONE',  ( -1.000000000000000000, 0.000000000000000000, 0.000000000000000000 ) ) ;
#1727 = CYLINDRICAL_SURFACE ( 'NONE', #9639, 27.60000000002759890 ) ;
#1728 = CIRCLE ( 'NONE', #11862, 23.00000000000000000 ) ;
#1729 = CARTESIAN_POINT ( 'NONE',  ( 6.250000000000054179, 10.82531754730546147, 129.0000000000000000 ) ) ;
#1730 = EDGE_CURVE ( 'NONE', #8987, #10156, #13632, .T. ) ;
#1731 = ORIENTED_EDGE ( 'NONE', *, *, #18227, .F. ) ;
#1732 = EDGE_CURVE ( 'NONE', #17728, #18597, #14993, .T. ) ;
#1733 = FACE_OUTER_BOUND ( 'NONE', #10053, .T. ) ;
#1734 = DIRECTION ( 'NONE',  ( -1.000000000000000000, -1.836909530733573776E-16, 0.000000000000000000 ) ) ;
#1735 = VECTOR ( 'NONE', #8612, 1000.000000000000000 ) ;
#1736 = DIRECTION ( 'NONE',  ( -1.000000000000000000, -0.000000000000000000, -0.000000000000000000 ) ) ;
#1737 = CARTESIAN_POINT ( 'NONE',  ( 50.00000000000000000, -172.4842959289096598, 69.62001590667014739 ) ) ;
#1738 = ORIENTED_EDGE ( 'NONE', *, *, #7506, .T. ) ;
#1739 = DIRECTION ( 'NONE',  ( -1.000000000000000000, 0.000000000000000000, 0.000000000000000000 ) ) ;
#1740 = EDGE_CURVE ( 'NONE', #200, #20371, #6508, .T. ) ;
#1741 = DIRECTION ( 'NONE',  ( -1.000000000000000000, -0.000000000000000000, -0.000000000000000000 ) ) ;
#1742 = CARTESIAN_POINT ( 'NONE',  ( 19.99999999999999645, 64.44931368725534071, -10.18420179740539666 ) ) ;
#1743 = ORIENTED_EDGE ( 'NONE', *, *, #9744, .F. ) ;
#1744 = DIRECTION ( 'NONE',  ( -1.000000000000000000, 0.000000000000000000, 0.000000000000000000 ) ) ;
#1745 = VERTEX_POINT ( 'NONE', #18821 ) ;
#1746 = FACE_OUTER_BOUND ( 'NONE', #19191, .T. ) ;
#1747 = VERTEX_POINT ( 'NONE', #19026 ) ;
#1748 = CIRCLE ( 'NONE', #16288, 8.500000000000000000 ) ;
#1749 = TOROIDAL_SURFACE ( 'NONE', #7480, 4.000000000000000000, 0.2500000000000000000 ) ;
#1750 = FACE_OUTER_BOUND ( 'NONE', #13395, .T. ) ;
#1751 = CARTESIAN_POINT ( 'NONE',  ( 9.999999999999998224, -70.68211945903199478, 13.71269443944183841 ) ) ;
#1752 = VECTOR ( 'NONE', #19396, 1000.000000000000000 ) ;
#1753 = CARTESIAN_POINT ( 'NONE',  ( 10.46442989454075700, 10.46442989202484419, -13.71283308115846111 ) ) ;
#1754 = ORIENTED_EDGE ( 'NONE', *, *, #11106, .T. ) ;
#1755 = FILL_AREA_STYLE ('',( #3737 ) ) ;
#1756 = CARTESIAN_POINT ( 'NONE',  ( 9.999999999999998224, -70.29359119158475266, -15.58239511117358589 ) ) ;
#1757 = ORIENTED_EDGE ( 'NONE', *, *, #3867, .T. ) ;
#1758 = AXIS2_PLACEMENT_3D ( 'NONE', #7578, #6086, #17759 ) ;
#1759 = DIRECTION ( 'NONE',  ( -1.000000000000000000, -0.000000000000000000, -0.000000000000000000 ) ) ;
#1760 = AXIS2_PLACEMENT_3D ( 'NONE', #5949, #17414, #4145 ) ;
#1761 = LINE ( 'NONE', #16378, #8504 ) ;
#1762 = AXIS2_PLACEMENT_3D ( 'NONE', #20211, #11949, #10154 ) ;
#1763 = DIRECTION ( 'NONE',  ( 1.000000000000000000, 0.000000000000000000, 0.000000000000000000 ) ) ;
#1764 = FACE_OUTER_BOUND ( 'NONE', #9147, .T. ) ;
#1765 = EDGE_LOOP ( 'NONE', ( #13180, #11942, #776, #17211 ) ) ;
#1766 = CARTESIAN_POINT ( 'NONE',  ( 19.99999999999999645, 43.56693332842786504, 48.57318520917521454 ) ) ;
#1767 = EDGE_LOOP ( 'NONE', ( #5370, #1113 ) ) ;
#1768 = SURFACE_STYLE_FILL_AREA ( #19880 ) ;
#1769 = CARTESIAN_POINT ( 'NONE',  ( 50.00000000000000000, 230.0000000000000000, 0.000000000000000000 ) ) ;
#1770 = CARTESIAN_POINT ( 'NONE',  ( 0.000000000000000000, 0.000000000000000000, -43.00000000000000000 ) ) ;
#1771 = ADVANCED_FACE ( 'NONE', ( #6192 ), #10770, .T. ) ;
#1772 = VERTEX_POINT ( 'NONE', #1237 ) ;
#1773 = CARTESIAN_POINT ( 'NONE',  ( 24.99999999999999645, -84.99999999999998579, -75.00000000000002842 ) ) ;
#1774 = CIRCLE ( 'NONE', #2443, 27.60000000002760245 ) ;
#1775 = CIRCLE ( 'NONE', #19362, 4.000000000000000888 ) ;
#1776 = CARTESIAN_POINT ( 'NONE',  ( -24.99999999999999289, -97.49621075554985339, -111.6458212409894486 ) ) ;
#1777 = VECTOR ( 'NONE', #541, 1000.000000000000000 ) ;
#1778 = CARTESIAN_POINT ( 'NONE',  ( 12.72792205982779912, -12.72792206288791483, -3.788324999819691286 ) ) ;
#1779 = ORIENTED_EDGE ( 'NONE', *, *, #5333, .F. ) ;
#1780 = PLANE ( 'NONE',  #10621 ) ;
#1781 = DIRECTION ( 'NONE',  ( -1.000000000000000000, 0.000000000000000000, -0.000000000000000000 ) ) ;
#1782 = CARTESIAN_POINT ( 'NONE',  ( 2.943691925285397470, -14.79893867793683349, -6.666073168480925126 ) ) ;
#1783 = CYLINDRICAL_SURFACE ( 'NONE', #7525, 5.000000000000000888 ) ;
#1784 = AXIS2_PLACEMENT_3D ( 'NONE', #16285, #15014, #13323 ) ;
#1785 = CIRCLE ( 'NONE', #4495, 27.60000000002759890 ) ;
#1786 = ORIENTED_EDGE ( 'NONE', *, *, #13103, .F. ) ;
#1787 = CARTESIAN_POINT ( 'NONE',  ( 45.76122707727121508, -127.3290820621008947, 85.00000000000000000 ) ) ;
#1788 = CARTESIAN_POINT ( 'NONE',  ( 4.248408730893249441, 6.358192987158596488, 24.01604375018031945 ) ) ;
#1789 = CARTESIAN_POINT ( 'NONE',  ( 33.60460458983040155, -28.85220587458695007, 68.11375585025291457 ) ) ;
#1790 = AXIS2_PLACEMENT_3D ( 'NONE', #4738, #6524, #17677 ) ;
#1791 = ORIENTED_EDGE ( 'NONE', *, *, #20113, .T. ) ;
#1792 = FACE_OUTER_BOUND ( 'NONE', #3371, .T. ) ;
#1793 = VERTEX_POINT ( 'NONE', #5987 ) ;
#1794 = CARTESIAN_POINT ( 'NONE',  ( 45.22159793441013420, -8.673994507468389514, -84.62946326583126222 ) ) ;
#1795 = CARTESIAN_POINT ( 'NONE',  ( 85.00002539999999840, 5.400000000000000355, -1.000000000000000000 ) ) ;
#1796 = EDGE_CURVE ( 'NONE', #4998, #13929, #18712, .T. ) ;
#1797 = EDGE_LOOP ( 'NONE', ( #3719, #7779, #12178, #4788 ) ) ;
#1798 = VECTOR ( 'NONE', #56, 1000.000000000000000 ) ;
#1799 =( BOUNDED_CURVE ( )  B_SPLINE_CURVE ( 2, ( #5374, #3882, #18309, #3775, #13232, #10257, #10052, #19790, #16516, #16719, #2000, #19989, #5272, #8658, #5472, #940, #2407 ),
 .UNSPECIFIED., .F., .T. ) 
 B_SPLINE_CURVE_WITH_KNOTS ( ( 3, 2, 2, 2, 2, 2, 2, 2, 3 ),
 ( 0.3000000000038511860, 0.3125000000038511971, 0.3250000000038512082, 0.3375000000038512193, 0.3500000000038511749, 0.3625000000038511860, 0.3750000000038511971, 0.3875000000038512082, 0.4000000000038512193 ),
 .UNSPECIFIED. ) 
 CURVE ( )  GEOMETRIC_REPRESENTATION_ITEM ( )  RATIONAL_B_SPLINE_CURVE ( ( 0.9999999999940800688, 0.9807852804091503618, 1.000000000000000000, 0.9807852804032304306, 1.000000000000000000, 0.9807852804032304306, 1.000000000000000000, 0.9807852804032304306, 1.000000000000000000, 0.9807852804032304306, 1.000000000000000000, 0.9807852804032304306, 1.000000000000000000, 0.9807852804032304306, 1.000000000000000000, 0.9807852803973104994, 1.000000000005919931 ) ) 
 REPRESENTATION_ITEM ( '' )  );
#1800 = ORIENTED_EDGE ( 'NONE', *, *, #5337, .F. ) ;
#1801 = FACE_OUTER_BOUND ( 'NONE', #11292, .T. ) ;
#1802 = FACE_OUTER_BOUND ( 'NONE', #15616, .T. ) ;
#1803 = SURFACE_STYLE_USAGE ( .BOTH. , #8258 ) ;
#1804 = DIRECTION ( 'NONE',  ( 0.000000000000000000, 0.000000000000000000, -1.000000000000000000 ) ) ;
#1805 = CIRCLE ( 'NONE', #15690, 27.60000000002759890 ) ;
#1806 = EDGE_CURVE ( 'NONE', #3529, #15394, #770, .T. ) ;
#1807 = AXIS2_PLACEMENT_3D ( 'NONE', #1341, #10861, #15626 ) ;
#1808 = CARTESIAN_POINT ( 'NONE',  ( 4.000000000000003553, -0.3902508023145564442, -1.995609623731131599E-15 ) ) ;
#1809 = CARTESIAN_POINT ( 'NONE',  ( -6.929096493489632635, 2.870125743571140919, 21.36526250018031803 ) ) ;
#1810 = CARTESIAN_POINT ( 'NONE',  ( -11.17563879758427525, -2.222972768810838051, -5.062141000286804804 ) ) ;
#1811 = AXIS2_PLACEMENT_3D ( 'NONE', #3048, #20476, #8226 ) ;
#1812 = DIRECTION ( 'NONE',  ( 1.000000000000000000, 0.000000000000000000, 0.000000000000000000 ) ) ;
#1813 = FACE_OUTER_BOUND ( 'NONE', #439, .T. ) ;
#1814 = EDGE_LOOP ( 'NONE', ( #19958, #17807 ) ) ;
#1815 = DIRECTION ( 'NONE',  ( 0.000000000000000000, 0.000000000000000000, 1.000000000000000000 ) ) ;
#1816 = CARTESIAN_POINT ( 'NONE',  ( 16.62983158603122291, 6.888301780572502864, 13.29448750018031511 ) ) ;
#1817 = CARTESIAN_POINT ( 'NONE',  ( 23.00000000000000000, 0.000000000000000000, -130.0000000000000000 ) ) ;
#1818 = VECTOR ( 'NONE', #4905, 1000.000000000000000 ) ;
#1819 = ORIENTED_EDGE ( 'NONE', *, *, #13003, .F. ) ;
#1820 = AXIS2_PLACEMENT_3D ( 'NONE', #15711, #20585, #1208 ) ;
#1821 = CARTESIAN_POINT ( 'NONE',  ( 4.000000000000003553, 2.309401076758480720, -5.599999999999999645 ) ) ;
#1822 = VERTEX_POINT ( 'NONE', #15941 ) ;
#1823 = DIRECTION ( 'NONE',  ( -1.000000000000000000, 0.000000000000000000, 0.000000000000000000 ) ) ;
#1824 = CARTESIAN_POINT ( 'NONE',  ( 30.00000000000000711, -49.00129691733391724, 71.78747447449033814 ) ) ;
#1825 = VERTEX_POINT ( 'NONE', #6298 ) ;
#1826 = ORIENTED_EDGE ( 'NONE', *, *, #8476, .T. ) ;
#1827 = DIRECTION ( 'NONE',  ( -1.000000000000000000, 0.000000000000000000, 0.000000000000000000 ) ) ;
#1828 = AXIS2_PLACEMENT_3D ( 'NONE', #19837, #10095, #11683 ) ;
#1829 = CARTESIAN_POINT ( 'NONE',  ( 3.345653888883671101, -2.687187980154741140, -0.1391502195351564664 ) ) ;
#1830 = AXIS2_PLACEMENT_3D ( 'NONE', #13244, #4984, #17710 ) ;
#1831 = EDGE_CURVE ( 'NONE', #1822, #15515, #1785, .T. ) ;
#1832 = EDGE_CURVE ( 'NONE', #1886, #19935, #4185, .T. ) ;
#1833 = DIRECTION ( 'NONE',  ( 1.000000000000000000, -0.000000000000000000, -0.000000000000000000 ) ) ;
#1834 = CIRCLE ( 'NONE', #4542, 27.60000000002759890 ) ;
#1835 = ORIENTED_EDGE ( 'NONE', *, *, #3908, .F. ) ;
#1836 = CARTESIAN_POINT ( 'NONE',  ( 5.303300858261582817, -5.303300859536631329, 10.97692500018031225 ) ) ;
#1837 = CARTESIAN_POINT ( 'NONE',  ( 0.000000000000000000, 64.80702306891106446, -7.581672767545749814 ) ) ;
#1838 = EDGE_CURVE ( 'NONE', #14211, #9376, #17446, .T. ) ;
#1839 = CYLINDRICAL_SURFACE ( 'NONE', #11990, 2.099999999999997868 ) ;
#1840 = CARTESIAN_POINT ( 'NONE',  ( -26.35784117651625280, 26.35784117651607872, -120.0000000000000142 ) ) ;
#1841 = ORIENTED_EDGE ( 'NONE', *, *, #12634, .T. ) ;
#1842 = CARTESIAN_POINT ( 'NONE',  ( 50.00000000000000000, -105.0000000000000000, -90.00000000000001421 ) ) ;
#1843 = EDGE_LOOP ( 'NONE', ( #9622, #15187, #15160, #5443, #19277 ) ) ;
#1844 = DIRECTION ( 'NONE',  ( 1.000000000000000000, 0.000000000000000000, 0.000000000000000000 ) ) ;
#1845 = CIRCLE ( 'NONE', #16054, 27.60000000002759890 ) ;
#1846 = ORIENTED_EDGE ( 'NONE', *, *, #13998, .T. ) ;
#1847 = DIRECTION ( 'NONE',  ( 0.000000000000000000, 1.000000000000000000, 0.000000000000000000 ) ) ;
#1848 = ORIENTED_EDGE ( 'NONE', *, *, #9782, .T. ) ;
#1849 = CARTESIAN_POINT ( 'NONE',  ( 19.99999999999999645, -63.85430960833482317, -11.25592921604904539 ) ) ;
#1850 = VERTEX_POINT ( 'NONE', #12560 ) ;
#1851 = EDGE_CURVE ( 'NONE', #4126, #9250, #2916, .T. ) ;
#1852 = DIRECTION ( 'NONE',  ( 1.000000000000000000, 0.000000000000000000, 0.000000000000000000 ) ) ;
#1853 = EDGE_CURVE ( 'NONE', #6239, #939, #2482, .T. ) ;
#1854 = EDGE_CURVE ( 'NONE', #5525, #20917, #15335, .T. ) ;
#1855 = CARTESIAN_POINT ( 'NONE',  ( 1.040949779275250179E-14, -85.00000000000000000, 5.000000000000000000 ) ) ;
#1856 = CARTESIAN_POINT ( 'NONE',  ( -10.32494394706616703, 4.276731815070943910, 2.944172250647428601 ) ) ;
#1857 = VERTEX_POINT ( 'NONE', #17557 ) ;
#1858 = EDGE_CURVE ( 'NONE', #7472, #2406, #12305, .T. ) ;
#1859 = VERTEX_POINT ( 'NONE', #1128 ) ;
#1860 = DIRECTION ( 'NONE',  ( 0.000000000000000000, 0.000000000000000000, 1.000000000000000000 ) ) ;
#1861 = AXIS2_PLACEMENT_3D ( 'NONE', #10011, #19864, #6928 ) ;
#1862 = ORIENTED_EDGE ( 'NONE', *, *, #14738, .T. ) ;
#1863 = ADVANCED_BREP_SHAPE_REPRESENTATION ( '', ( #17573, #12461 ), #3268 ) ;
#1864 = CARTESIAN_POINT ( 'NONE',  ( 6.888301780572507305, -16.62983158603121936, 15.65073750018031440 ) ) ;
#1865 = DIRECTION ( 'NONE',  ( -0.000000000000000000, -1.000000000000000000, -0.000000000000000000 ) ) ;
#1866 = CARTESIAN_POINT ( 'NONE',  ( 12.92641286132474931, -1.553915700095510638E-09, -21.87673848677710708 ) ) ;
#1867 = ORIENTED_EDGE ( 'NONE', *, *, #14885, .T. ) ;
#1868 = FACE_BOUND ( 'NONE', #1584, .T. ) ;
#1869 = AXIS2_PLACEMENT_3D ( 'NONE', #15664, #11001, #8431 ) ;
#1870 = VERTEX_POINT ( 'NONE', #9481 ) ;
#1871 = DIRECTION ( 'NONE',  ( -0.5000000000000037748, -0.8660254037844364872, 0.000000000000000000 ) ) ;
#1872 = EDGE_CURVE ( 'NONE', #6580, #9743, #15011, .T. ) ;
#1873 = CARTESIAN_POINT ( 'NONE',  ( 6.232799999999996565, 0.000000000000000000, 0.000000000000000000 ) ) ;
#1874 = ORIENTED_EDGE ( 'NONE', *, *, #17265, .T. ) ;
#1875 = DIRECTION ( 'NONE',  ( -1.000000000000000000, -0.000000000000000000, -0.000000000000000000 ) ) ;
#1876 = CARTESIAN_POINT ( 'NONE',  ( 2.500000000000000000, 0.000000000000000000, 0.000000000000000000 ) ) ;
#1877 = SHAPE_DEFINITION_REPRESENTATION ( #5771, #12383 ) ;
#1878 = CARTESIAN_POINT ( 'NONE',  ( -16.62983158437510411, 6.888301784570731279, -9.089887499819690575 ) ) ;
#1879 = ORIENTED_EDGE ( 'NONE', *, *, #3350, .F. ) ;
#1880 = CARTESIAN_POINT ( 'NONE',  ( 9.999999999999998224, 71.76067541710851572, 5.865617076724862322 ) ) ;
#1881 = CARTESIAN_POINT ( 'NONE',  ( -2.943691928843435779, -14.79893867722909917, 3.347989331519075851 ) ) ;
#1882 = EDGE_CURVE ( 'NONE', #9743, #10658, #20419, .T. ) ;
#1883 = AXIS2_PLACEMENT_3D ( 'NONE', #7227, #13709, #20157 ) ;
#1884 = CYLINDRICAL_SURFACE ( 'NONE', #8531, 3.199999999999994404 ) ;
#1885 = AXIS2_PLACEMENT_3D ( 'NONE', #10734, #17199, #2673 ) ;
#1886 = VERTEX_POINT ( 'NONE', #7576 ) ;
#1887 = CARTESIAN_POINT ( 'NONE',  ( 19.99999999999999645, 56.63599015375672963, 31.56633360682482703 ) ) ;
#1888 = CARTESIAN_POINT ( 'NONE',  ( 19.99999999999999645, 35.35772184876879720, 54.34979580218204376 ) ) ;
#1889 = CARTESIAN_POINT ( 'NONE',  ( 40.00000000000000711, 39.99999999999998579, -120.0000000000000142 ) ) ;
#1890 = ORIENTED_EDGE ( 'NONE', *, *, #6619, .F. ) ;
#1891 = CARTESIAN_POINT ( 'NONE',  ( 9.999999999999998224, 38.22257254261740655, 61.01667762370151848 ) ) ;
#1892 = ORIENTED_EDGE ( 'NONE', *, *, #16850, .F. ) ;
#1893 = DIRECTION ( 'NONE',  ( -1.000000000000000000, -0.000000000000000000, -0.000000000000000000 ) ) ;
#1894 = CARTESIAN_POINT ( 'NONE',  ( 12.72792206288790773, 12.72792205982779912, 20.22582500018031482 ) ) ;
#1895 = ORIENTED_EDGE ( 'NONE', *, *, #17550, .T. ) ;
#1896 = ORIENTED_EDGE ( 'NONE', *, *, #2354, .T. ) ;
#1897 = DIRECTION ( 'NONE',  ( -1.000000000000000000, 0.000000000000000000, 0.000000000000000000 ) ) ;
#1898 = COLOUR_RGB ( '', 0.66274510, 0.83137255, 0.94901961) ;
#1899 = AXIS2_PLACEMENT_3D ( 'NONE', #13062, #19519, #5306 ) ;
#1900 = FACE_OUTER_BOUND ( 'NONE', #18103, .T. ) ;
#1901 = PLANE ( 'NONE',  #13968 ) ;
#1902 = DIRECTION ( 'NONE',  ( -1.000000000000000000, -0.000000000000000000, 0.000000000000000000 ) ) ;
#1903 = AXIS2_PLACEMENT_3D ( 'NONE', #13104, #10660, #8951 ) ;
#1904 = AXIS2_PLACEMENT_3D ( 'NONE', #6518, #3652, #11608 ) ;
#1905 = CARTESIAN_POINT ( 'NONE',  ( -1.491842754445842800, 7.500000000179346316, 13.41291875018031554 ) ) ;
#1906 = CARTESIAN_POINT ( 'NONE',  ( -7.902369978624323110, -7.902369976724391343, -5.945734750286804093 ) ) ;
#1907 = EDGE_CURVE ( 'NONE', #281, #11746, #1147, .T. ) ;
#1908 = CIRCLE ( 'NONE', #10729, 10.52399999999999380 ) ;
#1909 = CYLINDRICAL_SURFACE ( 'NONE', #17185, 7.500000000000000000 ) ;
#1910 = CARTESIAN_POINT ( 'NONE',  ( 2.500000000000000000, -1.178949249685213863, 2.042000000000002924 ) ) ;
#1911 = AXIS2_PLACEMENT_3D ( 'NONE', #1216, #2688, #12441 ) ;
#1912 = EDGE_LOOP ( 'NONE', ( #92, #14154 ) ) ;
#1913 = DIRECTION ( 'NONE',  ( 0.000000000000000000, -0.5195839500354227924, -0.8544194045464950094 ) ) ;
#1914 = CIRCLE ( 'NONE', #3599, 11.17999999999999439 ) ;
#1915 = CARTESIAN_POINT ( 'NONE',  ( -16.62983158603122291, -6.888301780572501087, 18.00698750018031546 ) ) ;
#1916 = CARTESIAN_POINT ( 'NONE',  ( 30.00000000000000000, -85.00000000000000000, -1.040949779275250179E-14 ) ) ;
#1917 = ORIENTED_EDGE ( 'NONE', *, *, #14933, .F. ) ;
#1918 = CARTESIAN_POINT ( 'NONE',  ( 0.000000000000000000, -70.29359119158475266, -15.58239511117359299 ) ) ;
#1919 = CIRCLE ( 'NONE', #4279, 10.52399999999999558 ) ;
#1920 = ORIENTED_EDGE ( 'NONE', *, *, #19688, .T. ) ;
#1921 = CARTESIAN_POINT ( 'NONE',  ( 6.165579999999996730, 9.184850993605149917E-16, -7.500000000000001776 ) ) ;
#1922 = DIRECTION ( 'NONE',  ( 1.000000000000000000, 0.000000000000000000, 0.000000000000000000 ) ) ;
#1923 = ORIENTED_EDGE ( 'NONE', *, *, #9853, .T. ) ;
#1924 = ORIENTED_EDGE ( 'NONE', *, *, #1087, .F. ) ;
#1925 = DIRECTION ( 'NONE',  ( -0.000000000000000000, -0.000000000000000000, -1.000000000000000000 ) ) ;
#1926 = CIRCLE ( 'NONE', #5641, 10.00000000000000178 ) ;
#1927 =( LENGTH_UNIT ( ) NAMED_UNIT ( * ) SI_UNIT ( .MILLI., .METRE. ) );
#1928 = LINE ( 'NONE', #13270, #19772 ) ;
#1929 = CIRCLE ( 'NONE', #8356, 27.60000000002760956 ) ;
#1930 = DIRECTION ( 'NONE',  ( -1.000000000000000000, -0.000000000000000000, -0.000000000000000000 ) ) ;
#1931 = ORIENTED_EDGE ( 'NONE', *, *, #18504, .T. ) ;
#1932 = AXIS2_PLACEMENT_3D ( 'NONE', #8446, #11944, #15028 ) ;
#1933 = CARTESIAN_POINT ( 'NONE',  ( 4.248408729364575365, -6.358192988180014993, 11.27145625018031438 ) ) ;
#1934 = CIRCLE ( 'NONE', #1278, 2.500000000000000444 ) ;
#1935 = DIRECTION ( 'NONE',  ( -1.000000000000000000, 0.000000000000000000, 0.000000000000000000 ) ) ;
#1936 = DIRECTION ( 'NONE',  ( -1.000000000000000000, -0.000000000000000000, -0.000000000000000000 ) ) ;
#1937 = CARTESIAN_POINT ( 'NONE',  ( 19.99999999999999645, -14.55863677812078016, -63.60407295269120453 ) ) ;
#1938 = DIRECTION ( 'NONE',  ( 1.000000000000000000, 0.000000000000000000, 0.000000000000000000 ) ) ;
#1939 = ORIENTED_EDGE ( 'NONE', *, *, #522, .T. ) ;
#1940 = CARTESIAN_POINT ( 'NONE',  ( 50.00000000000000000, -110.0000000000000142, 44.99999999999999289 ) ) ;
#1941 = EDGE_LOOP ( 'NONE', ( #17646, #11307, #18490, #9324 ) ) ;
#1942 = CARTESIAN_POINT ( 'NONE',  ( 10.19618095414378800, 15.25966316918061416, 19.93129375018031268 ) ) ;
#1943 = LINE ( 'NONE', #3522, #14378 ) ;
#1944 = VECTOR ( 'NONE', #20097, 1000.000000000000000 ) ;
#1945 = ORIENTED_EDGE ( 'NONE', *, *, #16251, .F. ) ;
#1946 = EDGE_CURVE ( 'NONE', #12559, #405, #19541, .T. ) ;
#1947 = CYLINDRICAL_SURFACE ( 'NONE', #13320, 8.999999999999994671 ) ;
#1948 = EDGE_LOOP ( 'NONE', ( #19534, #18929, #17186, #3457, #542, #6703 ) ) ;
#1949 = LINE ( 'NONE', #45, #17304 ) ;
#1950 = DIRECTION ( 'NONE',  ( 0.000000000000000000, 0.000000000000000000, 1.000000000000000000 ) ) ;
#1951 = CIRCLE ( 'NONE', #13119, 20.00000000000000000 ) ;
#1952 = EDGE_CURVE ( 'NONE', #17356, #12057, #20748, .T. ) ;
#1953 = ORIENTED_EDGE ( 'NONE', *, *, #10892, .T. ) ;
#1954 = AXIS2_PLACEMENT_3D ( 'NONE', #11006, #17482, #10903 ) ;
#1955 = ADVANCED_FACE ( 'NONE', ( #12981 ), #9693, .T. ) ;
#1956 = CARTESIAN_POINT ( 'NONE',  ( -5.303300858261584594, 5.303300859536631329, -12.58557499981969130 ) ) ;
#1957 = PRESENTATION_STYLE_ASSIGNMENT (( #7928 ) ) ;
#1958 = FACE_OUTER_BOUND ( 'NONE', #4088, .T. ) ;
#1959 =( REPRESENTATION_RELATIONSHIP ('NONE','NONE', #13739, #2344 ) REPRESENTATION_RELATIONSHIP_WITH_TRANSFORMATION ( #1449 )SHAPE_REPRESENTATION_RELATIONSHIP( ) );
#1960 = CARTESIAN_POINT ( 'NONE',  ( -7.902369976724401113, 7.902369978624329327, 12.95823475064742780 ) ) ;
#1961 = ORIENTED_EDGE ( 'NONE', *, *, #12432, .T. ) ;
#1962 = DIRECTION ( 'NONE',  ( 0.000000000000000000, 0.000000000000000000, -1.000000000000000000 ) ) ;
#1963 = CIRCLE ( 'NONE', #6316, 27.60000000002760245 ) ;
#1964 = DIRECTION ( 'NONE',  ( 1.000000000000000000, -0.000000000000000000, -0.000000000000000000 ) ) ;
#1965 = EDGE_LOOP ( 'NONE', ( #16112, #3916 ) ) ;
#1966 = DIRECTION ( 'NONE',  ( -0.000000000000000000, -0.000000000000000000, 1.000000000000000000 ) ) ;
#1967 = ADVANCED_FACE ( 'NONE', ( #19435 ), #17863, .T. ) ;
#1968 = ORIENTED_EDGE ( 'NONE', *, *, #16242, .F. ) ;
#1969 = DIRECTION ( 'NONE',  ( -0.000000000000000000, -0.000000000000000000, 1.000000000000000000 ) ) ;
#1970 = CARTESIAN_POINT ( 'NONE',  ( 16.55500000000001393, 0.000000000000000000, 0.000000000000000000 ) ) ;
#1971 = DIRECTION ( 'NONE',  ( 0.000000000000000000, 1.000000000000000000, -1.471414886128461471E-15 ) ) ;
#1972 = EDGE_CURVE ( 'NONE', #15306, #1213, #5023, .T. ) ;
#1973 = EDGE_LOOP ( 'NONE', ( #407, #2959, #7904, #616 ) ) ;
#1974 = ADVANCED_FACE ( 'NONE', ( #11586 ), #11485, .F. ) ;
#1975 = CARTESIAN_POINT ( 'NONE',  ( 19.99999999999999645, 0.000000000000000000, 0.000000000000000000 ) ) ;
#1976 = ORIENTED_EDGE ( 'NONE', *, *, #19342, .F. ) ;
#1977 = CARTESIAN_POINT ( 'NONE',  ( 1.491842754445843688, -7.500000000179346316, -19.57458124981968695 ) ) ;
#1978 = ADVANCED_FACE ( 'NONE', ( #13186 ), #1947, .F. ) ;
#1979 = ADVANCED_FACE ( 'NONE', ( #9791 ), #9994, .F. ) ;
#1980 = EDGE_LOOP ( 'NONE', ( #1407, #18308 ) ) ;
#1981 = DIRECTION ( 'NONE',  ( -1.000000000000000000, 2.309263891220325289E-14, 0.000000000000000000 ) ) ;
#1982 = CARTESIAN_POINT ( 'NONE',  ( 19.99999999999999645, -5.762283366690708064, -64.99406197038676680 ) ) ;
#1983 = PRODUCT_CONTEXT ( 'NONE', #7900, 'mechanical' ) ;
#1984 = CARTESIAN_POINT ( 'NONE',  ( 5.663308646854342321, -13.67243654778935635, 8.082479418841543861 ) ) ;
#1985 = ORIENTED_EDGE ( 'NONE', *, *, #9043, .F. ) ;
#1986 = EDGE_CURVE ( 'NONE', #20036, #6207, #14480, .T. ) ;
#1987 = DIRECTION ( 'NONE',  ( 1.000000000000000000, 0.000000000000000000, 0.000000000000000000 ) ) ;
#1988 = ORIENTED_EDGE ( 'NONE', *, *, #10331, .T. ) ;
#1989 = EDGE_CURVE ( 'NONE', #6043, #14024, #14344, .T. ) ;
#1990 = CARTESIAN_POINT ( 'NONE',  ( 19.99999999999999645, -51.43306257653170377, 40.15061736769546741 ) ) ;
#1991 = EDGE_CURVE ( 'NONE', #3526, #20820, #8403, .T. ) ;
#1992 = CARTESIAN_POINT ( 'NONE',  ( 10.19618095414378622, 15.25966316918061239, 19.93129375018031268 ) ) ;
#1993 = ADVANCED_FACE ( 'NONE', ( #14874 ), #145, .T. ) ;
#1994 = DIRECTION ( 'NONE',  ( 0.000000000000000000, -0.5000000000000012212, -0.8660254037844380415 ) ) ;
#1995 = ORIENTED_EDGE ( 'NONE', *, *, #572, .T. ) ;
#1996 = EDGE_CURVE ( 'NONE', #3964, #14529, #6525, .T. ) ;
#1997 = CARTESIAN_POINT ( 'NONE',  ( 37.19682189084361568, -120.3881242644580709, 85.16117312608449197 ) ) ;
#1998 = DIRECTION ( 'NONE',  ( 1.000000000000000000, 0.000000000000000000, -0.000000000000000000 ) ) ;
#1999 = VERTEX_POINT ( 'NONE', #17648 ) ;
#2000 = CARTESIAN_POINT ( 'NONE',  ( 2.870125741905214412, -6.929096494179682431, 8.405887500180314831 ) ) ;
#2001 = ORIENTED_EDGE ( 'NONE', *, *, #13743, .F. ) ;
#2002 = CARTESIAN_POINT ( 'NONE',  ( 19.99999999999999645, -46.01927912072495275, -45.67597560296436399 ) ) ;
#2003 = CARTESIAN_POINT ( 'NONE',  ( 10.19618095414378622, 15.25966316918061239, 1.081293750180310820 ) ) ;
#2004 = ORIENTED_EDGE ( 'NONE', *, *, #18820, .T. ) ;
#2005 = VERTEX_POINT ( 'NONE', #3119 ) ;
#2006 = DIRECTION ( 'NONE',  ( -1.551631016079434660E-16, 1.000000000000000000, 0.000000000000000000 ) ) ;
#2007 = CARTESIAN_POINT ( 'NONE',  ( 0.000000000000000000, -36.59093685910587368, -62.00889726308067651 ) ) ;
#2008 = DIRECTION ( 'NONE',  ( 0.000000000000000000, -0.7812527682501556603, 0.6242147964454771714 ) ) ;
#2009 = CARTESIAN_POINT ( 'NONE',  ( -10.19618095414378800, -15.25966316918061771, 17.12339375018030907 ) ) ;
#2010 = UNCERTAINTY_MEASURE_WITH_UNIT (LENGTH_MEASURE( 1.000000000000000082E-05 ), #11516, 'distance_accuracy_value', 'NONE');
#2011 = CARTESIAN_POINT ( 'NONE',  ( 0.000000000000000000, 0.000000000000000000, 0.000000000000000000 ) ) ;
#2012 = CARTESIAN_POINT ( 'NONE',  ( 9.015937996181842420E-10, 7.500000000000007994, 23.13245000018031661 ) ) ;
#2013 = CARTESIAN_POINT ( 'NONE',  ( -11.17563879704981922, 2.222972771497742972, 4.951921499713198394 ) ) ;
#2014 = FACE_OUTER_BOUND ( 'NONE', #6061, .T. ) ;
#2015 = LINE ( 'NONE', #18328, #12395 ) ;
#2016 = VERTEX_POINT ( 'NONE', #12882 ) ;
#2017 = CYLINDRICAL_SURFACE ( 'NONE', #19701, 17.50000000000000355 ) ;
#2018 = CARTESIAN_POINT ( 'NONE',  ( -15.25966316918061771, 10.19618095414378622, 10.05464375018031475 ) ) ;
#2019 = FACE_BOUND ( 'NONE', #2437, .T. ) ;
#2020 = ORIENTED_EDGE ( 'NONE', *, *, #12147, .T. ) ;
#2021 = CARTESIAN_POINT ( 'NONE',  ( 2.500000000000000000, 1.178949249685213863, -2.042000000000001148 ) ) ;
#2022 = VECTOR ( 'NONE', #5978, 1000.000000000000000 ) ;
#2023 = ORIENTED_EDGE ( 'NONE', *, *, #19197, .F. ) ;
#2024 = FACE_OUTER_BOUND ( 'NONE', #1238, .T. ) ;
#2025 = CARTESIAN_POINT ( 'NONE',  ( 3.999999999999990674, -2.309401076758548221, -5.242734410091827613 ) ) ;
#2026 = ORIENTED_EDGE ( 'NONE', *, *, #7603, .F. ) ;
#2027 = VERTEX_POINT ( 'NONE', #19327 ) ;
#2028 = DIRECTION ( 'NONE',  ( -0.000000000000000000, -0.000000000000000000, -1.000000000000000000 ) ) ;
#2029 = ADVANCED_FACE ( 'NONE', ( #4813, #3225, #16163, #1655, #14574 ), #43, .F. ) ;
#2030 = CARTESIAN_POINT ( 'NONE',  ( 4.000000000000000000, 0.000000000000000000, 0.000000000000000000 ) ) ;
#2031 = CYLINDRICAL_SURFACE ( 'NONE', #1166, 65.24900000006525147 ) ;
#2032 = CARTESIAN_POINT ( 'NONE',  ( 7.500000000179339210, 1.491842754445841690, 18.92926875018031652 ) ) ;
#2033 = CARTESIAN_POINT ( 'NONE',  ( 30.51289089809370125, -109.5903380226954056, -78.78839954496530140 ) ) ;
#2034 = CARTESIAN_POINT ( 'NONE',  ( 19.99999999999999645, 0.000000000000000000, 0.000000000000000000 ) ) ;
#2035 = CARTESIAN_POINT ( 'NONE',  ( 19.99999999999999645, -31.98952867950364265, 56.39803944231574206 ) ) ;
#2036 = DIRECTION ( 'NONE',  ( -1.000000000000000000, 0.000000000000000000, 0.000000000000000000 ) ) ;
#2037 = ORIENTED_EDGE ( 'NONE', *, *, #2248, .F. ) ;
#2038 = DIRECTION ( 'NONE',  ( -0.000000000000000000, 0.000000000000000000, 1.000000000000000000 ) ) ;
#2039 = ORIENTED_EDGE ( 'NONE', *, *, #20622, .T. ) ;
#2040 = FACE_OUTER_BOUND ( 'NONE', #14555, .T. ) ;
#2041 = CARTESIAN_POINT ( 'NONE',  ( 19.99999999999999645, -51.96384592647234513, 49.83732252579596889 ) ) ;
#2042 = CIRCLE ( 'NONE', #4750, 27.60000000002759890 ) ;
#2043 = ORIENTED_EDGE ( 'NONE', *, *, #4432, .F. ) ;
#2044 = DIRECTION ( 'NONE',  ( -0.000000000000000000, -0.000000000000000000, 1.000000000000000000 ) ) ;
#2045 = ORIENTED_EDGE ( 'NONE', *, *, #14974, .T. ) ;
#2046 = PRODUCT_DEFINITION_SHAPE ( 'NONE', 'NONE',  #20956 ) ;
#2047 = CARTESIAN_POINT ( 'NONE',  ( 0.000000000000000000, -51.43306257653114955, -40.15061736769617795 ) ) ;
#2048 = DIRECTION ( 'NONE',  ( -1.000000000000000000, -0.000000000000000000, -0.000000000000000000 ) ) ;
#2049 = ORIENTED_EDGE ( 'NONE', *, *, #10414, .T. ) ;
#2050 = EDGE_CURVE ( 'NONE', #14215, #14337, #17033, .T. ) ;
#2051 = AXIS2_PLACEMENT_3D ( 'NONE', #20030, #8600, #15073 ) ;
#2052 = DIRECTION ( 'NONE',  ( 0.000000000000000000, -0.6310879443260593025, 0.7757112907044144690 ) ) ;
#2053 = CARTESIAN_POINT ( 'NONE',  ( 45.22159793441012710, -8.673994507468377080, 78.07221698934969822 ) ) ;
#2054 = AXIS2_PLACEMENT_3D ( 'NONE', #16360, #6804, #14876 ) ;
#2055 = CARTESIAN_POINT ( 'NONE',  ( -6.330490858644140850, -9.474249097082498849, 10.30745350064742993 ) ) ;
#2056 = EDGE_CURVE ( 'NONE', #405, #5157, #14981, .T. ) ;
#2057 = ORIENTED_EDGE ( 'NONE', *, *, #1831, .T. ) ;
#2058 = CARTESIAN_POINT ( 'NONE',  ( 19.99999999999999645, 42.42902769288536291, 49.02903636734212967 ) ) ;
#2059 = DIRECTION ( 'NONE',  ( 0.000000000000000000, 0.000000000000000000, -1.000000000000000000 ) ) ;
#2060 = EDGE_LOOP ( 'NONE', ( #7515, #17915, #1939, #1280 ) ) ;
#2061 = DIRECTION ( 'NONE',  ( 1.000000000000000000, 0.000000000000000000, 0.000000000000000000 ) ) ;
#2062 = ORIENTED_EDGE ( 'NONE', *, *, #8961, .T. ) ;
#2063 = CARTESIAN_POINT ( 'NONE',  ( 10.19618095414378800, 15.25966316918061416, 2.985893750180313777 ) ) ;
#2064 = DIRECTION ( 'NONE',  ( -0.000000000000000000, -0.000000000000000000, -1.000000000000000000 ) ) ;
#2065 = CARTESIAN_POINT ( 'NONE',  ( 2.500000000000000000, -1.178949249685214307, 2.042000000000001592 ) ) ;
#2066 = ADVANCED_FACE ( 'NONE', ( #18160 ), #3724, .T. ) ;
#2067 = VECTOR ( 'NONE', #1356, 1000.000000000000000 ) ;
#2068 = ORIENTED_EDGE ( 'NONE', *, *, #7031, .T. ) ;
#2069 = FACE_OUTER_BOUND ( 'NONE', #7501, .T. ) ;
#2070 = AXIS2_PLACEMENT_3D ( 'NONE', #17600, #19186, #15576 ) ;
#2071 = ORIENTED_EDGE ( 'NONE', *, *, #8027, .T. ) ;
#2072 = FACE_OUTER_BOUND ( 'NONE', #13430, .T. ) ;
#2073 = APPLICATION_CONTEXT ( 'automotive_design' ) ;
#2074 = ORIENTED_EDGE ( 'NONE', *, *, #17740, .F. ) ;
#2075 = AXIS2_PLACEMENT_3D ( 'NONE', #4773, #12945, #3081 ) ;
#2076 = CARTESIAN_POINT ( 'NONE',  ( 2.678494666091051801, 3.072372537026355044, -5.565789719053469753 ) ) ;
#2077 = DIRECTION ( 'NONE',  ( 0.000000000000000000, 0.000000000000000000, -1.000000000000000000 ) ) ;
#2078 = APPLICATION_PROTOCOL_DEFINITION ( 'draft international standard', 'automotive_design', 1998, #11824 ) ;
#2079 = CARTESIAN_POINT ( 'NONE',  ( 10.46442989202484064, -10.46442989454075878, 16.91841691884155452 ) ) ;
#2080 = AXIS2_PLACEMENT_3D ( 'NONE', #5832, #17194, #12523 ) ;
#2081 = EDGE_CURVE ( 'NONE', #11554, #20725, #11691, .T. ) ;
#2083 = ORIENTED_EDGE ( 'NONE', *, *, #7957, .T. ) ;
#2082 = CIRCLE ( 'NONE', #1068, 27.60000000002759535 ) ;
#2084 = EDGE_CURVE ( 'NONE', #15954, #13448, #5637, .T. ) ;
#2085 = CARTESIAN_POINT ( 'NONE',  ( 5.000000000000004441, 0.000000000000000000, 4.250000000000000000 ) ) ;
#2086 = AXIS2_PLACEMENT_3D ( 'NONE', #13971, #4530, #7604 ) ;
#2087 = CARTESIAN_POINT ( 'NONE',  ( -1.779019326032424095E-09, -14.79893867758296544, -25.22154191848092708 ) ) ;
#2088 = FACE_OUTER_BOUND ( 'NONE', #17108, .T. ) ;
#2089 = EDGE_CURVE ( 'NONE', #13866, #9669, #2359, .T. ) ;
#2090 = EDGE_CURVE ( 'NONE', #11808, #12431, #787, .T. ) ;
#2091 = ORIENTED_EDGE ( 'NONE', *, *, #730, .F. ) ;
#2092 = CARTESIAN_POINT ( 'NONE',  ( 30.00000000000000000, -105.0000000000000426, 77.45966692414833688 ) ) ;
#2093 = DIRECTION ( 'NONE',  ( -0.5000000000000051070, 0.000000000000000000, 0.8660254037844355990 ) ) ;
#2094 = ORIENTED_EDGE ( 'NONE', *, *, #17671, .T. ) ;
#2095 = CIRCLE ( 'NONE', #1106, 27.60000000002759890 ) ;
#2096 = DIRECTION ( 'NONE',  ( 1.000000000000000000, 1.836909530733573776E-16, 0.000000000000000000 ) ) ;
#2097 = VECTOR ( 'NONE', #11885, 1000.000000000000114 ) ;
#2098 = VERTEX_POINT ( 'NONE', #18582 ) ;
#2099 = FACE_OUTER_BOUND ( 'NONE', #7677, .T. ) ;
#2100 = CARTESIAN_POINT ( 'NONE',  ( 3.580422610670019878, -18.00000000043040771, 4.615668750180310198 ) ) ;
#2101 = ORIENTED_EDGE ( 'NONE', *, *, #16469, .T. ) ;
#2102 = CIRCLE ( 'NONE', #6500, 72.00000000007199219 ) ;
#2103 = EDGE_CURVE ( 'NONE', #2406, #13848, #19737, .T. ) ;
#2104 = VERTEX_POINT ( 'NONE', #4042 ) ;
#2105 = CYLINDRICAL_SURFACE ( 'NONE', #19854, 27.60000000002759890 ) ;
#2106 = ADVANCED_FACE ( 'NONE', ( #13594 ), #15281, .T. ) ;
#2107 = DIRECTION ( 'NONE',  ( -1.000000000000000000, 0.000000000000000000, 0.000000000000000000 ) ) ;
#2108 = DIRECTION ( 'NONE',  ( 0.7071067811865436870, 0.4413865154835798221, 0.5524291302504504841 ) ) ;
#2109 = DIRECTION ( 'NONE',  ( 0.000000000000000000, 0.000000000000000000, -1.000000000000000000 ) ) ;
#2110 = EDGE_CURVE ( 'NONE', #7909, #19902, #2462, .T. ) ;
#2111 = CARTESIAN_POINT ( 'NONE',  ( -24.99999999999999289, 230.0000000000000000, 0.000000000000000000 ) ) ;
#2112 = CARTESIAN_POINT ( 'NONE',  ( -2.870125743571144028, -6.929096493489630859, -9.265987499819688722 ) ) ;
#2113 = CIRCLE ( 'NONE', #419, 72.00000000007199219 ) ;
#2114 = CARTESIAN_POINT ( 'NONE',  ( -1.343452921478823292E-09, -11.17563879731704723, -7.123859750286805514 ) ) ;
#2115 = EDGE_CURVE ( 'NONE', #5814, #14337, #16026, .T. ) ;
#2116 = VECTOR ( 'NONE', #12051, 1000.000000000000000 ) ;
#2117 = AXIS2_PLACEMENT_3D ( 'NONE', #19356, #4841, #20632 ) ;
#2118 = DIRECTION ( 'NONE',  ( 0.000000000000000000, 0.000000000000000000, 1.000000000000000000 ) ) ;
#2119 = CARTESIAN_POINT ( 'NONE',  ( 1.660531772554325158, -3.660093687634888404, -5.599999999999981881 ) ) ;
#2120 = ORIENTED_EDGE ( 'NONE', *, *, #366, .F. ) ;
#2121 = CARTESIAN_POINT ( 'NONE',  ( 23.13963350654227824, -26.35784117651622793, -130.0000000000000000 ) ) ;
#2122 = CARTESIAN_POINT ( 'NONE',  ( 10.19618095047497874, -15.25966317163203279, -3.493793749819687822 ) ) ;
#2123 = FACE_BOUND ( 'NONE', #12789, .T. ) ;
#2124 = AXIS2_PLACEMENT_3D ( 'NONE', #16818, #3872, #703 ) ;
#2125 = ORIENTED_EDGE ( 'NONE', *, *, #3539, .F. ) ;
#2126 = CARTESIAN_POINT ( 'NONE',  ( 0.000000000000000000, 0.000000000000000000, 0.000000000000000000 ) ) ;
#2127 = ORIENTED_EDGE ( 'NONE', *, *, #6225, .F. ) ;
#2128 = DIRECTION ( 'NONE',  ( -0.000000000000000000, -0.000000000000000000, 1.000000000000000000 ) ) ;
#2129 = CARTESIAN_POINT ( 'NONE',  ( 0.000000000000000000, 43.56693332842852584, -48.57318520917462479 ) ) ;
#2130 = VERTEX_POINT ( 'NONE', #19941 ) ;
#2131 = ORIENTED_EDGE ( 'NONE', *, *, #7332, .T. ) ;
#2132 = LINE ( 'NONE', #15486, #10719 ) ;
#2133 = AXIS2_PLACEMENT_3D ( 'NONE', #1776, #11421, #6635 ) ;
#2134 = ADVANCED_FACE ( 'NONE', ( #19745 ), #3629, .F. ) ;
#2135 = AXIS2_PLACEMENT_3D ( 'NONE', #11722, #15010, #7046 ) ;
#2136 = CARTESIAN_POINT ( 'NONE',  ( 19.99999999999999645, 63.85430960833490843, 16.34407078397899582 ) ) ;
#2137 = LINE ( 'NONE', #5620, #15369 ) ;
#2138 = VECTOR ( 'NONE', #16410, 1000.000000000000000 ) ;
#2139 = CIRCLE ( 'NONE', #6535, 4.000000000000000000 ) ;
#2140 = CARTESIAN_POINT ( 'NONE',  ( 2.870125741905211747, -6.929096494179675325, 2.140987500180310921 ) ) ;
#2141 = CYLINDRICAL_SURFACE ( 'NONE', #2051, 2.099999999999997868 ) ;
#2142 =( LENGTH_UNIT ( ) NAMED_UNIT ( * ) SI_UNIT ( .MILLI., .METRE. ) );
#2143 = CIRCLE ( 'NONE', #7558, 27.60000000002760245 ) ;
#2144 = CYLINDRICAL_SURFACE ( 'NONE', #16598, 20.00000000000000355 ) ;
#2145 = FACE_OUTER_BOUND ( 'NONE', #6074, .T. ) ;
#2146 = ORIENTED_EDGE ( 'NONE', *, *, #554, .F. ) ;
#2147 = EDGE_CURVE ( 'NONE', #10416, #11011, #18051, .T. ) ;
#2148 = DIRECTION ( 'NONE',  ( -1.000000000000000000, -0.000000000000000000, -0.000000000000000000 ) ) ;
#2149 = VERTEX_POINT ( 'NONE', #10423 ) ;
#2150 = CARTESIAN_POINT ( 'NONE',  ( -3.580422614997675002, -17.99999999956958163, -4.220268749819688914 ) ) ;
#2151 = CARTESIAN_POINT ( 'NONE',  ( -10.58466049171560464, -18.71773173394922196, 71.82544846116155668 ) ) ;
#2152 = ORIENTED_EDGE ( 'NONE', *, *, #8330, .T. ) ;
#2153 = DIRECTION ( 'NONE',  ( -1.000000000000000000, 0.000000000000000000, 0.000000000000000000 ) ) ;
#2154 = ORIENTED_EDGE ( 'NONE', *, *, #19458, .F. ) ;
#2155 = DIRECTION ( 'NONE',  ( 0.000000000000000000, -0.7308359642781161458, -0.6825531432186624503 ) ) ;
#2156 = CARTESIAN_POINT ( 'NONE',  ( 0.000000000000000000, 0.000000000000000000, 46.00000000000000711 ) ) ;
#2157 = AXIS2_PLACEMENT_3D ( 'NONE', #10193, #18573, #656 ) ;
#2158 = ORIENTED_EDGE ( 'NONE', *, *, #783, .T. ) ;
#2159 = VECTOR ( 'NONE', #9655, 999.9999999999997726 ) ;
#2160 = VECTOR ( 'NONE', #14156, 1000.000000000000000 ) ;
#2161 = CARTESIAN_POINT ( 'NONE',  ( -6.929096493489627306, 2.870125743571138699, -13.17463749981969201 ) ) ;
#2162 = CARTESIAN_POINT ( 'NONE',  ( 12.72792205982779379, -12.72792206288790950, -5.692924999819690690 ) ) ;
#2163 = CIRCLE ( 'NONE', #474, 21.50000000000000000 ) ;
#2164 = CARTESIAN_POINT ( 'NONE',  ( 30.14578621226506172, -45.03195997035788167, -66.38288848018790134 ) ) ;
#2165 = AXIS2_PLACEMENT_3D ( 'NONE', #6082, #9274, #2700 ) ;
#2166 = DIRECTION ( 'NONE',  ( 1.000000000000000000, 0.000000000000000000, 0.000000000000000000 ) ) ;
#2167 = CARTESIAN_POINT ( 'NONE',  ( 6.330490858644141738, 9.474249097082498849, 15.01995350064743029 ) ) ;
#2168 = ORIENTED_EDGE ( 'NONE', *, *, #17652, .F. ) ;
#2169 = DIRECTION ( 'NONE',  ( 0.000000000000000000, -0.9790840876823249106, 0.2034560130526240906 ) ) ;
#2170 = CARTESIAN_POINT ( 'NONE',  ( 0.000000000000000000, -1.178949249685213863, 2.042000000000002924 ) ) ;
#2171 = ORIENTED_EDGE ( 'NONE', *, *, #5540, .F. ) ;
#2172 = CIRCLE ( 'NONE', #7587, 72.00000000007199219 ) ;
#2173 = CARTESIAN_POINT ( 'NONE',  ( -13.88581415360054550, -16.42997871820715616, -72.99065141121242561 ) ) ;
#2174 = ORIENTED_EDGE ( 'NONE', *, *, #19111, .F. ) ;
#2175 = EDGE_CURVE ( 'NONE', #9271, #10315, #13645, .T. ) ;
#2176 = CARTESIAN_POINT ( 'NONE',  ( -10.19618095047498052, 15.25966317163203101, 10.64370625018031369 ) ) ;
#2177 = LINE ( 'NONE', #16487, #4615 ) ;
#2178 = CARTESIAN_POINT ( 'NONE',  ( -7.500000000000000000, 0.000000000000000000, 40.00000000000000000 ) ) ;
#2179 = VECTOR ( 'NONE', #19320, 1000.000000000000000 ) ;
#2180 = VERTEX_POINT ( 'NONE', #3830 ) ;
#2181 = ORIENTED_EDGE ( 'NONE', *, *, #15321, .F. ) ;
#2182 = DIRECTION ( 'NONE',  ( -1.597351267013635531E-16, 1.000000000000000000, 0.000000000000000000 ) ) ;
#2183 = EDGE_LOOP ( 'NONE', ( #16569, #15786, #17436, #19964, #1862, #18536 ) ) ;
#2184 = LINE ( 'NONE', #10452, #7690 ) ;
#2185 = CARTESIAN_POINT ( 'NONE',  ( -52.00000000000000000, -39.99999999999999289, 5.000000000000000000 ) ) ;
#2186 = CARTESIAN_POINT ( 'NONE',  ( -10.46442989202484242, 10.46442989454075700, 12.20591691884154528 ) ) ;
#2187 = VERTEX_POINT ( 'NONE', #10202 ) ;
#2188 = CIRCLE ( 'NONE', #18440, 27.60000000002759890 ) ;
#2189 = LINE ( 'NONE', #13744, #13343 ) ;
#2190 = ORIENTED_EDGE ( 'NONE', *, *, #14380, .F. ) ;
#2191 = FACE_OUTER_BOUND ( 'NONE', #20815, .T. ) ;
#2192 = CARTESIAN_POINT ( 'NONE',  ( -14.79893867722910095, 2.943691928843434891, -22.57076066848093276 ) ) ;
#2193 = DIRECTION ( 'NONE',  ( 0.000000000000000000, 0.000000000000000000, 1.000000000000000000 ) ) ;
#2194 = DIRECTION ( 'NONE',  ( 0.000000000000000000, 0.9422609221188213979, -0.3348796121709835538 ) ) ;
#2195 = ORIENTED_EDGE ( 'NONE', *, *, #13247, .T. ) ;
#2196 = CARTESIAN_POINT ( 'NONE',  ( 30.50907704923281472, -109.5730600679726052, 78.78220139038879211 ) ) ;
#2197 = CARTESIAN_POINT ( 'NONE',  ( -7.500000000000002665, -4.022542205827308438E-17, 14.51130000000230602 ) ) ;
#2198 = ORIENTED_EDGE ( 'NONE', *, *, #20871, .T. ) ;
#2199 = CLOSED_SHELL ( 'NONE', ( #8939, #10001, #2881, #15044, #4425, #417, #1578, #445, #7289, #14821, #19003, #312, #11673, #4173, #5444, #9408, #16489, #13775, #2134, #6198, #11800, #19754, #8038, #11525, #887, #4962, #390 ) ) ;
#2200 = EDGE_CURVE ( 'NONE', #4444, #7461, #9248, .T. ) ;
#2201 = DIRECTION ( 'NONE',  ( 1.000000000000000000, -0.000000000000000000, -0.000000000000000000 ) ) ;
#2202 = ORIENTED_EDGE ( 'NONE', *, *, #9853, .F. ) ;
#2203 = CARTESIAN_POINT ( 'NONE',  ( 50.00000000000000000, 230.0000000000000000, -85.00000000000000000 ) ) ;
#2204 = CARTESIAN_POINT ( 'NONE',  ( -16.62983158437509701, 6.888301784570728614, 7.855512500180310553 ) ) ;
#2205 = EDGE_CURVE ( 'NONE', #520, #6509, #13499, .T. ) ;
#2206 = ORIENTED_EDGE ( 'NONE', *, *, #14142, .T. ) ;
#2207 = ORIENTED_EDGE ( 'NONE', *, *, #12482, .F. ) ;
#2208 = DIRECTION ( 'NONE',  ( -1.000000000000000000, -0.000000000000000000, 0.000000000000000000 ) ) ;
#2209 = FACE_OUTER_BOUND ( 'NONE', #14366, .T. ) ;
#2210 = DIRECTION ( 'NONE',  ( -1.000000000000000000, -1.836909530733573776E-16, 0.000000000000000000 ) ) ;
#2211 = EDGE_CURVE ( 'NONE', #1850, #5277, #5524, .T. ) ;
#2212 = CARTESIAN_POINT ( 'NONE',  ( -7.500000000000007105, 1.491842755816076505, -16.62926874991220672 ) ) ;
#2213 = UNCERTAINTY_MEASURE_WITH_UNIT (LENGTH_MEASURE( 1.000000000000000082E-05 ), #2484, 'distance_accuracy_value', 'NONE');
#2214 = CIRCLE ( 'NONE', #7634, 27.60000000002760245 ) ;
#2215 = FACE_OUTER_BOUND ( 'NONE', #8943, .T. ) ;
#2216 = CARTESIAN_POINT ( 'NONE',  ( -6.929096494179684207, -2.870125741905212635, 1.337137500180316074 ) ) ;
#2217 = CIRCLE ( 'NONE', #14082, 7.500000000000000000 ) ;
#2218 = CARTESIAN_POINT ( 'NONE',  ( -4.276731812588563386, 10.32494394809438987, -21.85042225028680818 ) ) ;
#2219 = DIRECTION ( 'NONE',  ( 0.000000000000000000, -0.8169698930104356549, -0.5766803221148764091 ) ) ;
#2220 = DIRECTION ( 'NONE',  ( -1.000000000000000000, 0.000000000000000000, -0.000000000000000000 ) ) ;
#2221 = ADVANCED_FACE ( 'NONE', ( #12212 ), #879, .T. ) ;
#2222 = ORIENTED_EDGE ( 'NONE', *, *, #4494, .F. ) ;
#2223 = CARTESIAN_POINT ( 'NONE',  ( 0.000000000000000000, 0.000000000000000000, 0.000000000000000000 ) ) ;
#2224 = CARTESIAN_POINT ( 'NONE',  ( 12.72792206288790950, 12.72792205982780089, 3.280425000180314132 ) ) ;
#2225 = CARTESIAN_POINT ( 'NONE',  ( 0.000000000000000000, 0.000000000000000000, 0.000000000000000000 ) ) ;
#2226 = EDGE_LOOP ( 'NONE', ( #10599, #3285, #1650, #3524 ) ) ;
#2227 = EDGE_CURVE ( 'NONE', #16282, #17758, #7202, .T. ) ;
#2228 = DIRECTION ( 'NONE',  ( -0.000000000000000000, -0.000000000000000000, 1.000000000000000000 ) ) ;
#2229 = ORIENTED_EDGE ( 'NONE', *, *, #14858, .F. ) ;
#2230 = DIRECTION ( 'NONE',  ( 1.000000000000000000, -0.000000000000000000, -0.000000000000000000 ) ) ;
#2231 = CARTESIAN_POINT ( 'NONE',  ( 0.000000000000000000, -1.971042061627920727, -64.80882494896108881 ) ) ;
#2232 = AXIS2_PLACEMENT_3D ( 'NONE', #17625, #11368, #11671 ) ;
#2233 = EDGE_CURVE ( 'NONE', #5012, #8902, #15023, .T. ) ;
#2234 = EDGE_LOOP ( 'NONE', ( #16109, #2711, #18909, #7545 ) ) ;
#2235 = VERTEX_POINT ( 'NONE', #7436 ) ;
#2236 = DIRECTION ( 'NONE',  ( 0.000000000000000000, 0.000000000000000000, 1.000000000000000000 ) ) ;
#2237 = VECTOR ( 'NONE', #6617, 1000.000000000000114 ) ;
#2238 = CIRCLE ( 'NONE', #4265, 72.00000000007199219 ) ;
#2239 = DIRECTION ( 'NONE',  ( -1.000000000000000000, -0.000000000000000000, 0.000000000000000000 ) ) ;
#2240 = AXIS2_PLACEMENT_3D ( 'NONE', #11200, #16463, #4634 ) ;
#2241 = DIRECTION ( 'NONE',  ( 0.000000000000000000, 0.000000000000000000, -1.000000000000000000 ) ) ;
#2242 = CARTESIAN_POINT ( 'NONE',  ( 7.500000000000000888, -9.015933403756337545E-10, -9.051199999819688813 ) ) ;
#2243 = VECTOR ( 'NONE', #19192, 1000.000000000000000 ) ;
#2244 = CARTESIAN_POINT ( 'NONE',  ( 30.06750564394959824, -106.8813891955586257, -77.91416960582807860 ) ) ;
#2245 = CARTESIAN_POINT ( 'NONE',  ( 0.000000000000000000, -24.01204443665145405, -60.22865198596149838 ) ) ;
#2246 = DIRECTION ( 'NONE',  ( 0.000000000000000000, 0.000000000000000000, -1.000000000000000000 ) ) ;
#2247 = FACE_OUTER_BOUND ( 'NONE', #14955, .T. ) ;
#2248 = EDGE_CURVE ( 'NONE', #20371, #8637, #5954, .T. ) ;
#2249 = VECTOR ( 'NONE', #8492, 1000.000000000000000 ) ;
#2250 = AXIS2_PLACEMENT_3D ( 'NONE', #11196, #10880, #14501 ) ;
#2251 = VERTEX_POINT ( 'NONE', #10743 ) ;
#2252 =( GEOMETRIC_REPRESENTATION_CONTEXT ( 3 ) GLOBAL_UNCERTAINTY_ASSIGNED_CONTEXT ( ( #16622 ) ) GLOBAL_UNIT_ASSIGNED_CONTEXT ( ( #20772, #1612, #12630 ) ) REPRESENTATION_CONTEXT ( 'NONE', 'WORKASPACE' ) );
#2253 = CARTESIAN_POINT ( 'NONE',  ( 0.000000000000000000, 0.000000000000000000, 126.0000000000000000 ) ) ;
#2254 = VERTEX_POINT ( 'NONE', #12326 ) ;
#2255 = CARTESIAN_POINT ( 'NONE',  ( 10.19618095047497874, -15.25966317163203279, -5.398393749819686782 ) ) ;
#2256 = DIRECTION ( 'NONE',  ( -1.000000000000000000, -0.000000000000000000, 0.000000000000000000 ) ) ;
#2257 = EDGE_LOOP ( 'NONE', ( #11256, #17039 ) ) ;
#2258 = CARTESIAN_POINT ( 'NONE',  ( 24.99999999999999289, -110.0000000000000142, 44.99999999999999289 ) ) ;
#2259 = ORIENTED_EDGE ( 'NONE', *, *, #8793, .T. ) ;
#2260 = CARTESIAN_POINT ( 'NONE',  ( 19.99999999999999645, 60.40676135667469282, -23.56039007468977431 ) ) ;
#2261 = FACE_OUTER_BOUND ( 'NONE', #4125, .T. ) ;
#2262 = EDGE_CURVE ( 'NONE', #18834, #7712, #10955, .T. ) ;
#2263 = CIRCLE ( 'NONE', #9361, 4.000000000000000888 ) ;
#2264 = ORIENTED_EDGE ( 'NONE', *, *, #11136, .T. ) ;
#2265 = AXIS2_PLACEMENT_3D ( 'NONE', #2535, #18317, #7071 ) ;
#2266 = AXIS2_PLACEMENT_3D ( 'NONE', #2316, #10476, #8769 ) ;
#2267 = CARTESIAN_POINT ( 'NONE',  ( -9.850000000000006750, 0.000000000000000000, -43.00000000000000000 ) ) ;
#2268 = CARTESIAN_POINT ( 'NONE',  ( 2.163825119083639120E-09, 17.99999999999999645, -9.227299999819690512 ) ) ;
#2269 = DIRECTION ( 'NONE',  ( -0.000000000000000000, -0.000000000000000000, 1.000000000000000000 ) ) ;
#2270 = AXIS2_PLACEMENT_3D ( 'NONE', #5785, #4208, #12376 ) ;
#2271 = CARTESIAN_POINT ( 'NONE',  ( -7.500000000000004441, 9.706494107352906755E-15, -4.338699999997692736 ) ) ;
#2272 = CARTESIAN_POINT ( 'NONE',  ( 11.17563879758428769, 2.222972768810838939, 16.19807850064743349 ) ) ;
#2273 = ORIENTED_EDGE ( 'NONE', *, *, #2295, .T. ) ;
#2274 =( LENGTH_UNIT ( ) NAMED_UNIT ( * ) SI_UNIT ( .MILLI., .METRE. ) );
#2275 = CARTESIAN_POINT ( 'NONE',  ( 0.000000000000000000, 0.000000000000000000, -68.00000000000000000 ) ) ;
#2276 = ORIENTED_EDGE ( 'NONE', *, *, #4160, .T. ) ;
#2277 = CARTESIAN_POINT ( 'NONE',  ( 4.119954785698654476, -21.10500016855060679, -70.74589478160186218 ) ) ;
#2278 = ORIENTED_EDGE ( 'NONE', *, *, #15463, .T. ) ;
#2279 = AXIS2_PLACEMENT_3D ( 'NONE', #4218, #17157, #20433 ) ;
#2280 = CARTESIAN_POINT ( 'NONE',  ( -3.580422614997675002, -17.99999999956958163, -2.315668749819689065 ) ) ;
#2281 = CARTESIAN_POINT ( 'NONE',  ( 0.000000000000000000, -53.26727847779572045, 48.44168704307611506 ) ) ;
#2282 = CARTESIAN_POINT ( 'NONE',  ( 50.00000000000000000, -160.0000000000000000, 0.000000000000000000 ) ) ;
#2283 = EDGE_LOOP ( 'NONE', ( #8472, #7507, #18183, #15740 ) ) ;
#2284 = AXIS2_PLACEMENT_3D ( 'NONE', #17168, #15669, #2652 ) ;
#2285 = CARTESIAN_POINT ( 'NONE',  ( -32.96694501150314949, -24.74873734152930993, -120.0000000000000142 ) ) ;
#2286 = ORIENTED_EDGE ( 'NONE', *, *, #20426, .T. ) ;
#2287 = CARTESIAN_POINT ( 'NONE',  ( -2.870125741905213079, 6.929096494179683319, 13.11838750018031519 ) ) ;
#2288 = AXIS2_PLACEMENT_3D ( 'NONE', #6398, #4606, #10858 ) ;
#2289 = ORIENTED_EDGE ( 'NONE', *, *, #19061, .F. ) ;
#2290 = DIRECTION ( 'NONE',  ( -1.000000000000000000, -0.000000000000000000, -0.000000000000000000 ) ) ;
#2291 = AXIS2_PLACEMENT_3D ( 'NONE', #19254, #8406, #5330 ) ;
#2292 = VERTEX_POINT ( 'NONE', #9249 ) ;
#2293 = CYLINDRICAL_SURFACE ( 'NONE', #8724, 7.500000000000000000 ) ;
#2294 = EDGE_CURVE ( 'NONE', #6278, #12115, #6540, .T. ) ;
#2295 = EDGE_CURVE ( 'NONE', #16235, #5869, #6885, .T. ) ;
#2296 = CIRCLE ( 'NONE', #945, 34.99999999999999289 ) ;
#2297 = DIRECTION ( 'NONE',  ( 1.000000000000000000, -0.000000000000000000, -0.000000000000000000 ) ) ;
#2298 = CONTEXT_DEPENDENT_SHAPE_REPRESENTATION ( #1170, #5079 ) ;
#2299 = CARTESIAN_POINT ( 'NONE',  ( -5.663308650141539502, -13.67243654642775574, 9.260604418841545282 ) ) ;
#2300 = ORIENTED_EDGE ( 'NONE', *, *, #631, .F. ) ;
#2301 = CARTESIAN_POINT ( 'NONE',  ( 6.249999999999902300, -10.82531754730554496, 43.00000000000000000 ) ) ;
#2302 = VERTEX_POINT ( 'NONE', #17419 ) ;
#2303 = CARTESIAN_POINT ( 'NONE',  ( 6.249999999999902300, -10.82531754730554496, 40.00000000000000000 ) ) ;
#2304 = CARTESIAN_POINT ( 'NONE',  ( 5.663308650141530620, 13.67243654642775041, -19.91997941848093490 ) ) ;
#2305 = CARTESIAN_POINT ( 'NONE',  ( 19.99999999999999645, 54.08351995568756365, -35.76369202524444546 ) ) ;
#2306 = VERTEX_POINT ( 'NONE', #14232 ) ;
#2307 = DIRECTION ( 'NONE',  ( -1.000000000000000000, 0.000000000000000000, 0.000000000000000000 ) ) ;
#2308 = CARTESIAN_POINT ( 'NONE',  ( 1.491842756249029289, 7.499999999820664343, 17.16208125018031083 ) ) ;
#2309 = EDGE_LOOP ( 'NONE', ( #16752, #9506 ) ) ;
#2310 = DIRECTION ( 'NONE',  ( 0.000000000000000000, 0.000000000000000000, 1.000000000000000000 ) ) ;
#2311 = ORIENTED_EDGE ( 'NONE', *, *, #10468, .F. ) ;
#2312 = DIRECTION ( 'NONE',  ( -1.000000000000000000, -0.000000000000000000, 0.000000000000000000 ) ) ;
#2313 = CARTESIAN_POINT ( 'NONE',  ( -3.580422610670017658, 18.00000000043040771, -0.09683124981969132294 ) ) ;
#2314 = VERTEX_POINT ( 'NONE', #18793 ) ;
#2315 = ORIENTED_EDGE ( 'NONE', *, *, #16854, .T. ) ;
#2316 = CARTESIAN_POINT ( 'NONE',  ( 5.200000000000002842, 0.000000000000000000, -2.700000000000000622 ) ) ;
#2317 = FACE_OUTER_BOUND ( 'NONE', #17971, .T. ) ;
#2318 = PLANE ( 'NONE',  #7168 ) ;
#2319 = FACE_OUTER_BOUND ( 'NONE', #14479, .T. ) ;
#2320 = CARTESIAN_POINT ( 'NONE',  ( 19.99999999999999645, 46.01927912072526539, 45.67597560296404424 ) ) ;
#2321 = CARTESIAN_POINT ( 'NONE',  ( -6.358192987158596488, 4.248408730893249441, 2.809793750180315186 ) ) ;
#2322 = CARTESIAN_POINT ( 'NONE',  ( 9.999999999999998224, -59.36728637277992249, -40.73727173906846843 ) ) ;
#2323 = EDGE_CURVE ( 'NONE', #15053, #11776, #13664, .T. ) ;
#2324 = CARTESIAN_POINT ( 'NONE',  ( -10.32494394706615815, 4.276731815070940357, -13.60354725028680356 ) ) ;
#2325 = DIRECTION ( 'NONE',  ( 1.000000000000000000, 1.836909530733573776E-16, 0.000000000000000000 ) ) ;
#2326 = VERTEX_POINT ( 'NONE', #4263 ) ;
#2327 = LINE ( 'NONE', #16742, #14309 ) ;
#2328 = CARTESIAN_POINT ( 'NONE',  ( -17.99999999956958519, 3.580422614997674113, 0.04058125018031183417 ) ) ;
#2329 = DIRECTION ( 'NONE',  ( -1.000000000000000000, 0.000000000000000000, 0.000000000000000000 ) ) ;
#2330 = EDGE_CURVE ( 'NONE', #11776, #11750, #17206, .T. ) ;
#2331 = ORIENTED_EDGE ( 'NONE', *, *, #20367, .F. ) ;
#2332 = EDGE_CURVE ( 'NONE', #20245, #15954, #19753, .T. ) ;
#2333 = LINE ( 'NONE', #18133, #7581 ) ;
#2334 = ORIENTED_EDGE ( 'NONE', *, *, #20490, .T. ) ;
#2335 = CARTESIAN_POINT ( 'NONE',  ( -31.35784117651625635, 26.35784117651607872, -120.0000000000000142 ) ) ;
#2336 = DIRECTION ( 'NONE',  ( -1.000000000000000000, -0.000000000000000000, -0.000000000000000000 ) ) ;
#2337 = ORIENTED_EDGE ( 'NONE', *, *, #19059, .T. ) ;
#2338 = ORIENTED_EDGE ( 'NONE', *, *, #11165, .F. ) ;
#2339 = CARTESIAN_POINT ( 'NONE',  ( 0.000000000000000000, 0.000000000000000000, 0.000000000000000000 ) ) ;
#2340 = AXIS2_PLACEMENT_3D ( 'NONE', #5183, #8072, #16017 ) ;
#2341 = PRESENTATION_STYLE_ASSIGNMENT (( #17191 ) ) ;
#2342 = FACE_BOUND ( 'NONE', #2460, .T. ) ;
#2343 = DIRECTION ( 'NONE',  ( -1.000000000000000000, 0.000000000000000000, 0.000000000000000000 ) ) ;
#2344 = SHAPE_REPRESENTATION ( 'hex nut gradec_iso_ISO - 4034 - M5 - N', ( #12461 ), #12750 ) ;
#2345 = EDGE_CURVE ( 'NONE', #10694, #11336, #1315, .T. ) ;
#2346 = CARTESIAN_POINT ( 'NONE',  ( -7.500000000000000888, 9.015942588607330751E-10, -13.76369999981968917 ) ) ;
#2347 = EDGE_CURVE ( 'NONE', #3334, #8219, #11626, .T. ) ;
#2348 = DIRECTION ( 'NONE',  ( 0.000000000000000000, 0.000000000000000000, 1.000000000000000000 ) ) ;
#2349 = DIRECTION ( 'NONE',  ( 0.000000000000000000, 0.8660254037844380415, -0.5000000000000012212 ) ) ;
#2350 = PLANE ( 'NONE',  #15362 ) ;
#2351 = ORIENTED_EDGE ( 'NONE', *, *, #18142, .T. ) ;
#2352 = CARTESIAN_POINT ( 'NONE',  ( 19.99999999999999645, 44.69367065308644271, 56.44887778834761605 ) ) ;
#2353 = ORIENTED_EDGE ( 'NONE', *, *, #15535, .T. ) ;
#2354 = EDGE_CURVE ( 'NONE', #5060, #5564, #1507, .T. ) ;
#2355 = CARTESIAN_POINT ( 'NONE',  ( -10.19618095047498052, 15.25966317163203101, -0.6858937498196854277 ) ) ;
#2356 = CARTESIAN_POINT ( 'NONE',  ( -65.00002539999999840, 0.000000000000000000, -7.500000000000000000 ) ) ;
#2357 = ORIENTED_EDGE ( 'NONE', *, *, #4699, .T. ) ;
#2358 = PRODUCT_DEFINITION ( 'UNKNOWN', '', #4244, #17267 ) ;
#2359 = LINE ( 'NONE', #15186, #4858 ) ;
#2360 = EDGE_LOOP ( 'NONE', ( #18552, #13909 ) ) ;
#2361 = DIRECTION ( 'NONE',  ( -1.000000000000000000, -0.000000000000000000, -0.000000000000000000 ) ) ;
#2362 = DIRECTION ( 'NONE',  ( -1.000000000000000000, 0.000000000000000000, 0.000000000000000000 ) ) ;
#2363 = ORIENTED_EDGE ( 'NONE', *, *, #18967, .F. ) ;
#2364 = PLANE ( 'NONE',  #1883 ) ;
#2365 = EDGE_CURVE ( 'NONE', #9313, #2489, #17527, .T. ) ;
#2366 = CARTESIAN_POINT ( 'NONE',  ( 9.015937996181835182E-10, 7.500000000000002665, -11.40744999981969166 ) ) ;
#2367 = CARTESIAN_POINT ( 'NONE',  ( -12.72792206288790950, -12.72792205982779556, -3.336674999819690068 ) ) ;
#2368 = CARTESIAN_POINT ( 'NONE',  ( -4.000000000000000000, -0.7779732554280792689, -0.03354435108167819896 ) ) ;
#2369 = ADVANCED_FACE ( 'NONE', ( #13817 ), #9455, .T. ) ;
#2370 = CARTESIAN_POINT ( 'NONE',  ( -6.929096494179678878, -2.870125741905209971, 13.92223750018030870 ) ) ;
#2371 = CARTESIAN_POINT ( 'NONE',  ( 10.32494394809439875, 4.276731812588567827, -2.946452749352572287 ) ) ;
#2372 = ORIENTED_EDGE ( 'NONE', *, *, #16212, .F. ) ;
#2373 = DIRECTION ( 'NONE',  ( 0.000000000000000000, 0.000000000000000000, -1.000000000000000000 ) ) ;
#2374 = ADVANCED_FACE ( 'NONE', ( #18904 ), #4152, .T. ) ;
#2375 = CYLINDRICAL_SURFACE ( 'NONE', #9838, 2.649999999999993694 ) ;
#2376 = EDGE_LOOP ( 'NONE', ( #8040, #13146, #1073, #324 ) ) ;
#2377 = CARTESIAN_POINT ( 'NONE',  ( 3.744012722225332990, -21.17498532244396969, -70.71631193418077999 ) ) ;
#2378 = EDGE_LOOP ( 'NONE', ( #1879, #14922 ) ) ;
#2379 = CARTESIAN_POINT ( 'NONE',  ( -10.19618095414378622, -15.25966316918061416, 7.698393750180313688 ) ) ;
#2380 = DIRECTION ( 'NONE',  ( -0.000000000000000000, 0.8660254037844390407, 0.4999999999999993339 ) ) ;
#2381 = DIRECTION ( 'NONE',  ( 0.000000000000000000, 0.000000000000000000, -1.000000000000000000 ) ) ;
#2382 = ORIENTED_EDGE ( 'NONE', *, *, #17265, .F. ) ;
#2383 = DIRECTION ( 'NONE',  ( 1.000000000000000000, 0.000000000000000000, 0.000000000000000000 ) ) ;
#2384 = ORIENTED_EDGE ( 'NONE', *, *, #5532, .F. ) ;
#2385 = LINE ( 'NONE', #9170, #12249 ) ;
#2386 = AXIS2_PLACEMENT_3D ( 'NONE', #20275, #14362, #11377 ) ;
#2387 = EDGE_LOOP ( 'NONE', ( #10662, #11563, #2719, #10655 ) ) ;
#2388 = CARTESIAN_POINT ( 'NONE',  ( -10.00000000000000000, 0.000000000000000000, 0.000000000000000000 ) ) ;
#2389 = VECTOR ( 'NONE', #8302, 1000.000000000000000 ) ;
#2390 = ORIENTED_EDGE ( 'NONE', *, *, #8242, .T. ) ;
#2391 = DIRECTION ( 'NONE',  ( 1.000000000000000000, 0.000000000000000000, 0.000000000000000000 ) ) ;
#2392 = PRODUCT_DEFINITION_SHAPE ( 'NONE', 'NONE',  #20945 ) ;
#2393 = DIRECTION ( 'NONE',  ( -1.000000000000000000, -0.000000000000000000, -0.000000000000000000 ) ) ;
#2394 = CONTEXT_DEPENDENT_SHAPE_REPRESENTATION ( #11310, #12397 ) ;
#2395 = CARTESIAN_POINT ( 'NONE',  ( 8.382925371439633011, 12.54593441562640876, 14.26763566884154777 ) ) ;
#2396 = VERTEX_POINT ( 'NONE', #14030 ) ;
#2397 = AXIS2_PLACEMENT_3D ( 'NONE', #679, #16899, #790 ) ;
#2398 = DIRECTION ( 'NONE',  ( -1.000000000000000000, -0.000000000000000000, -0.000000000000000000 ) ) ;
#2399 = CARTESIAN_POINT ( 'NONE',  ( 19.99999999999999645, 0.000000000000000000, 0.000000000000000000 ) ) ;
#2400 = CARTESIAN_POINT ( 'NONE',  ( -2.943691928843435779, -14.79893867722909917, -24.92701066848092850 ) ) ;
#2401 = CARTESIAN_POINT ( 'NONE',  ( -25.00000000000000000, -30.00000000000000711, 58.09475019311124555 ) ) ;
#2402 = EDGE_LOOP ( 'NONE', ( #17842, #5849 ) ) ;
#2403 = EDGE_CURVE ( 'NONE', #2438, #12530, #13333, .T. ) ;
#2404 = CARTESIAN_POINT ( 'NONE',  ( 31.31307953385777054, -112.1412981899224519, 79.85379371982303098 ) ) ;
#2405 = CARTESIAN_POINT ( 'NONE',  ( 0.2500000000000002220, 0.000000000000000000, 4.250000000000000000 ) ) ;
#2406 = VERTEX_POINT ( 'NONE', #9670 ) ;
#2407 = CARTESIAN_POINT ( 'NONE',  ( 7.500000000000007105, 4.207617034055637320E-15, 6.638700000002313750 ) ) ;
#2408 = VERTEX_POINT ( 'NONE', #17835 ) ;
#2409 = DIRECTION ( 'NONE',  ( -1.000000000000000000, -0.000000000000000000, -0.000000000000000000 ) ) ;
#2410 = CARTESIAN_POINT ( 'NONE',  ( -2.163827323447877821E-09, -17.99999999999999645, 4.910200000180310553 ) ) ;
#2411 = EDGE_LOOP ( 'NONE', ( #5675, #4612, #5419, #5529 ) ) ;
#2412 = ORIENTED_EDGE ( 'NONE', *, *, #20065, .T. ) ;
#2413 = CARTESIAN_POINT ( 'NONE',  ( 19.99999999999999645, -60.40676135667420965, -23.56039007469101421 ) ) ;
#2414 = VECTOR ( 'NONE', #14278, 1000.000000000000000 ) ;
#2415 = CARTESIAN_POINT ( 'NONE',  ( -25.39999999999999858, 0.000000000000000000, 0.000000000000000000 ) ) ;
#2416 = DIRECTION ( 'NONE',  ( -1.000000000000000000, 0.000000000000000000, 0.000000000000000000 ) ) ;
#2417 = CIRCLE ( 'NONE', #7157, 65.24900000006526568 ) ;
#2418 =( NAMED_UNIT ( * ) SI_UNIT ( $, .STERADIAN. ) SOLID_ANGLE_UNIT ( ) );
#2419 = CARTESIAN_POINT ( 'NONE',  ( -10.19618095047498230, 15.25966317163203279, 20.06870625018031262 ) ) ;
#2420 = UNCERTAINTY_MEASURE_WITH_UNIT (LENGTH_MEASURE( 1.000000000000000082E-05 ), #14805, 'distance_accuracy_value', 'NONE');
#2421 = CARTESIAN_POINT ( 'NONE',  ( 2.870125743571140475, 6.929096493489632635, -4.553487499819687478 ) ) ;
#2422 = VECTOR ( 'NONE', #9660, 1000.000000000000000 ) ;
#2423 = CARTESIAN_POINT ( 'NONE',  ( 4.248408729364579806, -6.358192988180021210, 17.53635625018031519 ) ) ;
#2424 = CARTESIAN_POINT ( 'NONE',  ( -10.32494394706615815, 4.276731815070940357, -23.02854725028680960 ) ) ;
#2425 = DIRECTION ( 'NONE',  ( 0.000000000000000000, 0.000000000000000000, -1.000000000000000000 ) ) ;
#2426 = ORIENTED_EDGE ( 'NONE', *, *, #18690, .F. ) ;
#2427 = ADVANCED_FACE ( 'NONE', ( #14450 ), #9862, .T. ) ;
#2428 = CARTESIAN_POINT ( 'NONE',  ( 0.6554360035617794455, -4.240386000424091861, -0.1586754815285204845 ) ) ;
#2429 = CARTESIAN_POINT ( 'NONE',  ( -3.580422614997675002, -17.99999999956958163, -2.315668749819689065 ) ) ;
#2430 = DIRECTION ( 'NONE',  ( 0.000000000000000000, 0.000000000000000000, 1.000000000000000000 ) ) ;
#2431 = AXIS2_PLACEMENT_3D ( 'NONE', #5821, #12297, #18770 ) ;
#2432 = ORIENTED_EDGE ( 'NONE', *, *, #14802, .F. ) ;
#2433 = CARTESIAN_POINT ( 'NONE',  ( 0.000000000000000000, 0.000000000000000000, 0.000000000000000000 ) ) ;
#2434 = ORIENTED_EDGE ( 'NONE', *, *, #13718, .F. ) ;
#2435 = DIRECTION ( 'NONE',  ( -1.000000000000000000, 0.000000000000000000, 0.000000000000000000 ) ) ;
#2436 = FACE_OUTER_BOUND ( 'NONE', #5477, .T. ) ;
#2437 = EDGE_LOOP ( 'NONE', ( #5886, #5732 ) ) ;
#2438 = VERTEX_POINT ( 'NONE', #19510 ) ;
#2439 = CARTESIAN_POINT ( 'NONE',  ( 19.99999999999999645, -63.85430960833482317, -11.25592921604904539 ) ) ;
#2440 = EDGE_CURVE ( 'NONE', #10418, #12190, #4876, .T. ) ;
#2441 = SHAPE_REPRESENTATION_RELATIONSHIP ( 'NONE' , 'NONE' ,  #13064, #19794 ) ;
#2442 = CARTESIAN_POINT ( 'NONE',  ( 9.999999999999998224, -68.15657073222419626, -23.20952102120350702 ) ) ;
#2443 = AXIS2_PLACEMENT_3D ( 'NONE', #3785, #17737, #12863 ) ;
#2444 = VECTOR ( 'NONE', #18332, 1000.000000000000000 ) ;
#2445 = CIRCLE ( 'NONE', #14311, 39.99999999999999289 ) ;
#2446 = CYLINDRICAL_SURFACE ( 'NONE', #2515, 27.60000000002760245 ) ;
#2447 = AXIS2_PLACEMENT_3D ( 'NONE', #514, #18421, #13544 ) ;
#2448 = CARTESIAN_POINT ( 'NONE',  ( 1.491842756249028845, 7.499999999820661678, -1.687918749819689035 ) ) ;
#2449 = FACE_OUTER_BOUND ( 'NONE', #14624, .T. ) ;
#2450 = DIRECTION ( 'NONE',  ( 1.000000000000000000, -0.000000000000000000, -0.000000000000000000 ) ) ;
#2451 = CIRCLE ( 'NONE', #18370, 27.60000000002759535 ) ;
#2452 = CARTESIAN_POINT ( 'NONE',  ( 0.000000000000000000, -31.17893654894190902, -57.31758819669202865 ) ) ;
#2453 = CARTESIAN_POINT ( 'NONE',  ( 9.999999999999998224, 67.51707036274413554, 25.00890260772400708 ) ) ;
#2454 = ORIENTED_EDGE ( 'NONE', *, *, #15088, .T. ) ;
#2455 = DIRECTION ( 'NONE',  ( -1.000000000000000000, 0.000000000000000000, 0.000000000000000000 ) ) ;
#2456 = VERTEX_POINT ( 'NONE', #16330 ) ;
#2457 = CARTESIAN_POINT ( 'NONE',  ( -12.72792205982779912, 12.72792206288790950, -0.9804249998196858940 ) ) ;
#2458 = DIRECTION ( 'NONE',  ( 0.000000000000000000, 0.000000000000000000, 1.000000000000000000 ) ) ;
#2459 = CIRCLE ( 'NONE', #14327, 2.649999999999993694 ) ;
#2460 = EDGE_LOOP ( 'NONE', ( #20784, #5794 ) ) ;
#2461 = AXIS2_PLACEMENT_3D ( 'NONE', #20283, #17008, #3365 ) ;
#2462 = LINE ( 'NONE', #2258, #7559 ) ;
#2463 = ORIENTED_EDGE ( 'NONE', *, *, #10375, .F. ) ;
#2464 = COLOUR_RGB ( '', 0.40784314, 0.44705882, 0.49803922) ;
#2465 = CARTESIAN_POINT ( 'NONE',  ( 24.99999999999999289, -29.99999999999999645, -45.00000000000000000 ) ) ;
#2466 = CARTESIAN_POINT ( 'NONE',  ( 0.000000000000000000, 0.000000000000000000, -81.99999999999998579 ) ) ;
#2467 = CARTESIAN_POINT ( 'NONE',  ( -11.49999999999998934, -85.00000000000000000, 19.00000000000000000 ) ) ;
#2468 = STYLED_ITEM ( 'NONE', ( #11505 ), #3497 ) ;
#2469 = EDGE_LOOP ( 'NONE', ( #20521, #11520 ) ) ;
#2470 = CARTESIAN_POINT ( 'NONE',  ( 2.500000000000000000, 2.357898499370431722, -2.818925648462311528E-15 ) ) ;
#2471 = ADVANCED_FACE ( 'NONE', ( #6682 ), #14640, .F. ) ;
#2472 = EDGE_CURVE ( 'NONE', #14189, #4504, #8918, .T. ) ;
#2473 =( BOUNDED_CURVE ( )  B_SPLINE_CURVE ( 2, ( #20035, #8712, #16766, #10417, #13587, #5321, #344, #6797, #16877, #5519, #19841, #20142, #763, #3518, #7107, #11998, #5632 ),
 .UNSPECIFIED., .F., .F. ) 
 B_SPLINE_CURVE_WITH_KNOTS ( ( 3, 2, 2, 2, 2, 2, 2, 2, 3 ),
 ( 0.4000000000038512193, 0.4125000000038511749, 0.4250000000038511860, 0.4375000000038511971, 0.4500000000038512082, 0.4625000000038511638, 0.4750000000038511194, 0.4875000000038511305, 0.5000000000038511416 ),
 .UNSPECIFIED. ) 
 CURVE ( )  GEOMETRIC_REPRESENTATION_ITEM ( )  RATIONAL_B_SPLINE_CURVE ( ( 0.9999999999940800688, 0.9807852804091503618, 1.000000000000000000, 0.9807852804032304306, 1.000000000000000000, 0.9807852804032304306, 1.000000000000000000, 0.9807852804032304306, 1.000000000000000000, 0.9807852804032304306, 1.000000000000000000, 0.9807852804032304306, 1.000000000000000000, 0.9807852804032304306, 1.000000000000000000, 0.9807852803973104994, 1.000000000005919931 ) ) 
 REPRESENTATION_ITEM ( '' )  );
#2474 = VECTOR ( 'NONE', #15517, 1000.000000000000000 ) ;
#2475 = CARTESIAN_POINT ( 'NONE',  ( 19.99999999999999645, 59.31169354540775629, -27.19476070466793871 ) ) ;
#2476 = CARTESIAN_POINT ( 'NONE',  ( 18.00000000043040771, 3.580422610670018546, -7.165581249819690690 ) ) ;
#2477 = CARTESIAN_POINT ( 'NONE',  ( 19.99999999999999645, 0.000000000000000000, 0.000000000000000000 ) ) ;
#2478 = AXIS2_PLACEMENT_3D ( 'NONE', #18141, #6476, #16545 ) ;
#2479 = ADVANCED_FACE ( 'NONE', ( #4999 ), #11361, .T. ) ;
#2480 = CARTESIAN_POINT ( 'NONE',  ( -2.222972771497745192, -11.17563879704982632, -9.131608999352575751 ) ) ;
#2481 = CIRCLE ( 'NONE', #18048, 8.999999999999998224 ) ;
#2483 = ORIENTED_EDGE ( 'NONE', *, *, #20515, .T. ) ;
#2482 = CIRCLE ( 'NONE', #14664, 65.24900000006526568 ) ;
#2484 =( LENGTH_UNIT ( ) NAMED_UNIT ( * ) SI_UNIT ( .MILLI., .METRE. ) );
#2485 = CARTESIAN_POINT ( 'NONE',  ( 8.899999999999890221, -10.82531754730554496, 46.00000000000000711 ) ) ;
#2487 = EDGE_LOOP ( 'NONE', ( #9117, #16079, #3978, #3865, #20366 ) ) ;
#2486 = APPLICATION_CONTEXT ( 'automotive_design' ) ;
#2488 = CARTESIAN_POINT ( 'NONE',  ( 30.00000000000000000, 4.299168419249259188, -84.99999999999998579 ) ) ;
#2489 = VERTEX_POINT ( 'NONE', #8273 ) ;
#2490 = CARTESIAN_POINT ( 'NONE',  ( -6.888301784570738384, -16.62983158437509346, 7.403862500180314221 ) ) ;
#2491 = CYLINDRICAL_SURFACE ( 'NONE', #13076, 63.70999227554992217 ) ;
#2492 = DIRECTION ( 'NONE',  ( 1.000000000000000000, 0.000000000000000000, 0.000000000000000000 ) ) ;
#2493 = AXIS2_PLACEMENT_3D ( 'NONE', #15387, #16874, #7323 ) ;
#2494 = VERTEX_POINT ( 'NONE', #18028 ) ;
#2495 = AXIS2_PLACEMENT_3D ( 'NONE', #3186, #8365, #1613 ) ;
#2496 = EDGE_CURVE ( 'NONE', #19685, #17353, #4136, .T. ) ;
#2497 = DIRECTION ( 'NONE',  ( 0.000000000000000000, 0.000000000000000000, 1.000000000000000000 ) ) ;
#2498 = ORIENTED_EDGE ( 'NONE', *, *, #1580, .T. ) ;
#2499 = CARTESIAN_POINT ( 'NONE',  ( -7.500000000000007105, -3.289131931996631318E-15, 11.35120000000231677 ) ) ;
#2500 = EDGE_LOOP ( 'NONE', ( #17069, #5268, #8184, #2039 ) ) ;
#2501 = CARTESIAN_POINT ( 'NONE',  ( -30.00000000000000000, 36.35083268962915781, -50.00000000000000000 ) ) ;
#2502 = AXIS2_PLACEMENT_3D ( 'NONE', #6469, #13161, #11251 ) ;
#2503 = EDGE_CURVE ( 'NONE', #15688, #8604, #17730, .T. ) ;
#2504 = ADVANCED_FACE ( 'NONE', ( #4895 ), #3308, .T. ) ;
#2505 = CARTESIAN_POINT ( 'NONE',  ( 19.99999999999999645, 0.000000000000000000, 0.000000000000000000 ) ) ;
#2506 = EDGE_CURVE ( 'NONE', #15181, #11708, #9611, .T. ) ;
#2507 = DIRECTION ( 'NONE',  ( 1.000000000000000000, 0.000000000000000000, 0.000000000000000000 ) ) ;
#2508 = APPLICATION_PROTOCOL_DEFINITION ( 'draft international standard', 'automotive_design', 1998, #13591 ) ;
#2509 = VECTOR ( 'NONE', #15178, 1000.000000000000000 ) ;
#2510 = CARTESIAN_POINT ( 'NONE',  ( 1.779017513685136568E-09, 14.79893867758297610, 3.959041918841544216 ) ) ;
#2511 = VECTOR ( 'NONE', #20879, 1000.000000000000000 ) ;
#2512 = ORIENTED_EDGE ( 'NONE', *, *, #9952, .T. ) ;
#2513 = CYLINDRICAL_SURFACE ( 'NONE', #3801, 17.50000000000000355 ) ;
#2514 = ORIENTED_EDGE ( 'NONE', *, *, #5799, .T. ) ;
#2515 = AXIS2_PLACEMENT_3D ( 'NONE', #7099, #19929, #18246 ) ;
#2516 = CARTESIAN_POINT ( 'NONE',  ( -7.056982170014208577, -20.35833373244388511, 76.58484614278654590 ) ) ;
#2517 = CARTESIAN_POINT ( 'NONE',  ( -3.580422614997674557, -17.99999999956957808, 5.204731250180311797 ) ) ;
#2518 = AXIS2_PLACEMENT_3D ( 'NONE', #9789, #3223, #1653 ) ;
#2519 = CYLINDRICAL_SURFACE ( 'NONE', #385, 5.000000000000000888 ) ;
#2520 = ADVANCED_FACE ( 'NONE', ( #6377 ), #11556, .T. ) ;
#2521 = VERTEX_POINT ( 'NONE', #14345 ) ;
#2522 = CYLINDRICAL_SURFACE ( 'NONE', #20546, 72.00000000007199219 ) ;
#2523 = CARTESIAN_POINT ( 'NONE',  ( -30.00000000000000000, -85.00000000000000000, -14.50000000000000533 ) ) ;
#2524 = AXIS2_PLACEMENT_3D ( 'NONE', #580, #20270, #10531 ) ;
#2525 = ORIENTED_EDGE ( 'NONE', *, *, #19695, .F. ) ;
#2526 = CARTESIAN_POINT ( 'NONE',  ( -9.591132434872761792, -20.91852224714069663, -76.31448437082826786 ) ) ;
#2527 = EDGE_LOOP ( 'NONE', ( #15680, #10668 ) ) ;
#2528 = DIRECTION ( 'NONE',  ( 0.6156453966108028641, 0.000000000000000000, 0.7880233154113698291 ) ) ;
#2529 = CARTESIAN_POINT ( 'NONE',  ( -12.72792206288790950, -12.72792205982779556, -12.76167499981969300 ) ) ;
#2530 = VERTEX_POINT ( 'NONE', #19300 ) ;
#2531 = ORIENTED_EDGE ( 'NONE', *, *, #4934, .T. ) ;
#2532 = DIRECTION ( 'NONE',  ( 1.000000000000000000, 0.000000000000000000, 0.000000000000000000 ) ) ;
#2533 = AXIS2_PLACEMENT_3D ( 'NONE', #3699, #8469, #7192 ) ;
#2534 = CARTESIAN_POINT ( 'NONE',  ( 19.99999999999999645, -63.85430960833497949, 11.25592921604817676 ) ) ;
#2535 = CARTESIAN_POINT ( 'NONE',  ( -10.00000000000000000, 0.000000000000000000, 0.000000000000000000 ) ) ;
#2536 = CARTESIAN_POINT ( 'NONE',  ( -7.500000000000009770, 9.706494107251932559E-15, -16.92379999999768359 ) ) ;
#2537 = CARTESIAN_POINT ( 'NONE',  ( -6.888301780572502864, 16.62983158603122646, 1.513237500180307560 ) ) ;
#2538 = EDGE_CURVE ( 'NONE', #16575, #17634, #20790, .T. ) ;
#2539 = CARTESIAN_POINT ( 'NONE',  ( -8.500000000000000000, 1.040949779275250140E-15, 81.99999999999998579 ) ) ;
#2540 = CARTESIAN_POINT ( 'NONE',  ( -7.500000000179346316, -1.491842754445844355, -7.793331249819686057 ) ) ;
#2541 = MECHANICAL_DESIGN_GEOMETRIC_PRESENTATION_REPRESENTATION (  '', ( #20852 ), #12048 ) ;
#2542 = CARTESIAN_POINT ( 'NONE',  ( -6.929096494179684207, -2.870125741905212635, 20.18713750018031305 ) ) ;
#2543 = CARTESIAN_POINT ( 'NONE',  ( 6.330490858644138186, 9.474249097082495297, -10.95276600028680569 ) ) ;
#2544 = CIRCLE ( 'NONE', #3219, 72.00000000007199219 ) ;
#2545 = CARTESIAN_POINT ( 'NONE',  ( 0.000000000000000000, 0.000000000000000000, 166.0000000000000000 ) ) ;
#2546 = EDGE_LOOP ( 'NONE', ( #18740, #19824, #13697, #8968, #17911 ) ) ;
#2547 = CARTESIAN_POINT ( 'NONE',  ( 7.500000000000007105, -2.290195989506637665E-15, 16.06370000000231357 ) ) ;
#2548 = CARTESIAN_POINT ( 'NONE',  ( -10.19618095047498052, 15.25966317163203101, 1.218706250180314088 ) ) ;
#2549 = CARTESIAN_POINT ( 'NONE',  ( 30.00000000000000000, -122.0000000000000000, -6.368163355566234804E-15 ) ) ;
#2550 = ORIENTED_EDGE ( 'NONE', *, *, #14654, .T. ) ;
#2551 = CARTESIAN_POINT ( 'NONE',  ( 0.000000000000000000, 1.971042061629218356, -64.80882494896104618 ) ) ;
#2552 = ORIENTED_EDGE ( 'NONE', *, *, #14792, .F. ) ;
#2553 = CARTESIAN_POINT ( 'NONE',  ( 0.000000000000000000, 0.000000000000000000, 0.000000000000000000 ) ) ;
#2554 = PLANE ( 'NONE',  #1595 ) ;
#2555 = ORIENTED_EDGE ( 'NONE', *, *, #3243, .F. ) ;
#2556 = VERTEX_POINT ( 'NONE', #12758 ) ;
#2557 = VERTEX_POINT ( 'NONE', #19783 ) ;
#2558 = DIRECTION ( 'NONE',  ( 0.000000000000000000, 0.000000000000000000, 1.000000000000000000 ) ) ;
#2559 = SURFACE_SIDE_STYLE ('',( #4246 ) ) ;
#2560 = PLANE ( 'NONE',  #9591 ) ;
#2561 = EDGE_CURVE ( 'NONE', #11740, #6167, #4690, .T. ) ;
#2562 = EDGE_CURVE ( 'NONE', #7334, #17345, #3822, .T. ) ;
#2563 = DIRECTION ( 'NONE',  ( 0.000000000000000000, 0.9976687691905390398, 0.06824241336467466723 ) ) ;
#2564 = CARTESIAN_POINT ( 'NONE',  ( 9.015937996181834148E-10, 7.500000000000000888, -11.40744999981968810 ) ) ;
#2565 = CARTESIAN_POINT ( 'NONE',  ( 0.000000000000000000, 2.357898499370433054, -1.951563910473907981E-15 ) ) ;
#2566 = DIRECTION ( 'NONE',  ( 0.000000000000000000, 0.000000000000000000, 1.000000000000000000 ) ) ;
#2567 = DIRECTION ( 'NONE',  ( 0.000000000000000000, -0.000000000000000000, 1.000000000000000000 ) ) ;
#2568 = DIRECTION ( 'NONE',  ( 0.000000000000000000, 0.000000000000000000, 1.000000000000000000 ) ) ;
#2569 = ORIENTED_EDGE ( 'NONE', *, *, #1609, .T. ) ;
#2570 = DIRECTION ( 'NONE',  ( -1.000000000000000000, 0.000000000000000000, 0.000000000000000000 ) ) ;
#2571 = VECTOR ( 'NONE', #15402, 1000.000000000000000 ) ;
#2572 = ORIENTED_EDGE ( 'NONE', *, *, #20490, .F. ) ;
#2573 = CARTESIAN_POINT ( 'NONE',  ( -6.888301780572501976, 16.62983158603122291, -0.3913624998196884031 ) ) ;
#2574 = CARTESIAN_POINT ( 'NONE',  ( 0.6949845910673706495, -21.50225451306873481, 70.57937617215436887 ) ) ;
#2575 = ORIENTED_EDGE ( 'NONE', *, *, #9724, .F. ) ;
#2576 = DIRECTION ( 'NONE',  ( 0.000000000000000000, 0.000000000000000000, -1.000000000000000000 ) ) ;
#2577 = ORIENTED_EDGE ( 'NONE', *, *, #13101, .F. ) ;
#2578 = AXIS2_PLACEMENT_3D ( 'NONE', #20888, #9762, #9663 ) ;
#2579 = CARTESIAN_POINT ( 'NONE',  ( 50.00000000000000000, -29.99999999999999645, -45.00000000000000000 ) ) ;
#2580 = DIRECTION ( 'NONE',  ( -1.000000000000000000, -0.000000000000000000, 0.000000000000000000 ) ) ;
#2581 = DIRECTION ( 'NONE',  ( -1.000000000000000000, -0.000000000000000000, -0.000000000000000000 ) ) ;
#2582 = ORIENTED_EDGE ( 'NONE', *, *, #14780, .T. ) ;
#2583 = CARTESIAN_POINT ( 'NONE',  ( 2.870125741905214412, -6.929096494179682431, -19.86911249981968552 ) ) ;
#2584 = LINE ( 'NONE', #10646, #10427 ) ;
#2585 = CARTESIAN_POINT ( 'NONE',  ( 15.25966316918061239, -10.19618095414378445, -24.83745624981969513 ) ) ;
#2586 = CARTESIAN_POINT ( 'NONE',  ( 0.000000000000000000, 1.178949249685213863, -2.042000000000001148 ) ) ;
#2587 =( GEOMETRIC_REPRESENTATION_CONTEXT ( 3 ) GLOBAL_UNCERTAINTY_ASSIGNED_CONTEXT ( ( #18321 ) ) GLOBAL_UNIT_ASSIGNED_CONTEXT ( ( #13661, #7498, #2418 ) ) REPRESENTATION_CONTEXT ( 'NONE', 'WORKASPACE' ) );
#2588 = AXIS2_PLACEMENT_3D ( 'NONE', #13797, #12303, #20341 ) ;
#2589 = DIRECTION ( 'NONE',  ( -1.000000000000000000, -0.000000000000000000, -0.000000000000000000 ) ) ;
#2590 = EDGE_LOOP ( 'NONE', ( #8518, #519, #2101, #6155, #17013 ) ) ;
#2591 = AXIS2_PLACEMENT_3D ( 'NONE', #9741, #90, #6750 ) ;
#2592 = AXIS2_PLACEMENT_3D ( 'NONE', #20669, #17198, #983 ) ;
#2593 = CARTESIAN_POINT ( 'NONE',  ( 19.99999999999999645, -29.55812890831937878, -65.65300461859717984 ) ) ;
#2594 = EDGE_LOOP ( 'NONE', ( #3421, #12271 ) ) ;
#2595 = CARTESIAN_POINT ( 'NONE',  ( -11.54691128655043642, -18.15138880902595275, -72.10074112616624120 ) ) ;
#2596 = CARTESIAN_POINT ( 'NONE',  ( -7.500000000000007105, 1.491842755816076505, -7.204268749912206893 ) ) ;
#2597 = EDGE_CURVE ( 'NONE', #15726, #9191, #19090, .T. ) ;
#2598 = EDGE_LOOP ( 'NONE', ( #5245, #15939, #1097, #5912 ) ) ;
#2599 = B_SPLINE_CURVE_WITH_KNOTS ( 'NONE', 3,
 ( #10966, #4713, #10768, #12558 ),
 .UNSPECIFIED., .F., .F.,
 ( 4, 4 ),
 ( 2.380737581618737539E-07, 0.002336974151641576809 ),
 .UNSPECIFIED. ) ;
#2600 = EDGE_CURVE ( 'NONE', #20455, #2408, #2333, .T. ) ;
#2601 = CARTESIAN_POINT ( 'NONE',  ( 17.99999999956958163, -3.580422614997676334, -14.09691874981968951 ) ) ;
#2602 = CIRCLE ( 'NONE', #13781, 27.60000000002759890 ) ;
#2603 = PLANE ( 'NONE',  #13126 ) ;
#2604 = LINE ( 'NONE', #4063, #19513 ) ;
#2605 = ORIENTED_EDGE ( 'NONE', *, *, #11547, .T. ) ;
#2606 = CARTESIAN_POINT ( 'NONE',  ( 9.999999999999998224, -64.36139404985986801, 32.27399814043853610 ) ) ;
#2607 = AXIS2_PLACEMENT_3D ( 'NONE', #17816, #13039, #3379 ) ;
#2608 = VERTEX_POINT ( 'NONE', #3603 ) ;
#2609 = CARTESIAN_POINT ( 'NONE',  ( 0.000000000000000000, 0.000000000000000000, 68.00000000000000000 ) ) ;
#2610 = EDGE_CURVE ( 'NONE', #12500, #16359, #15355, .T. ) ;
#2611 = EDGE_LOOP ( 'NONE', ( #8358, #15861, #18578, #20131 ) ) ;
#2612 = EDGE_CURVE ( 'NONE', #7632, #18559, #15691, .T. ) ;
#2613 = CYLINDRICAL_SURFACE ( 'NONE', #16848, 27.60000000002760245 ) ;
#2614 = CARTESIAN_POINT ( 'NONE',  ( 2.500000000000000000, 1.178949249685212974, -2.042000000000001148 ) ) ;
#2615 = VECTOR ( 'NONE', #18973, 1000.000000000000000 ) ;
#2616 = CARTESIAN_POINT ( 'NONE',  ( 13.67243654642775574, -5.663308650141541278, 6.904354418841546881 ) ) ;
#2617 = EDGE_CURVE ( 'NONE', #13626, #14401, #18446, .T. ) ;
#2618 = ORIENTED_EDGE ( 'NONE', *, *, #522, .F. ) ;
#2619 = VECTOR ( 'NONE', #13322, 1000.000000000000000 ) ;
#2620 = DIRECTION ( 'NONE',  ( 1.000000000000000000, 0.000000000000000000, 0.000000000000000000 ) ) ;
#2621 = VERTEX_POINT ( 'NONE', #15257 ) ;
#2622 = CARTESIAN_POINT ( 'NONE',  ( -16.85739145898632074, -13.40013307497100925, 80.75697659352094604 ) ) ;
#2623 = EDGE_CURVE ( 'NONE', #6843, #8495, #20078, .T. ) ;
#2624 = AXIS2_PLACEMENT_3D ( 'NONE', #20264, #15399, #10130 ) ;
#2625 = CARTESIAN_POINT ( 'NONE',  ( 17.99999999956957808, -3.580422614997675446, 12.27348125018031055 ) ) ;
#2626 = AXIS2_PLACEMENT_3D ( 'NONE', #532, #2325, #6979 ) ;
#2627 = ADVANCED_FACE ( 'NONE', ( #13679 ), #13370, .F. ) ;
#2628 = DIRECTION ( 'NONE',  ( 0.000000000000000000, 0.000000000000000000, 1.000000000000000000 ) ) ;
#2629 = CARTESIAN_POINT ( 'NONE',  ( 0.3263565795980685191, -4.430380094434308802, -5.351519936624961282 ) ) ;
#2630 = ORIENTED_EDGE ( 'NONE', *, *, #11328, .F. ) ;
#2631 = EDGE_CURVE ( 'NONE', #2098, #7589, #9928, .T. ) ;
#2632 = DIRECTION ( 'NONE',  ( -1.000000000000000000, 0.000000000000000000, 0.000000000000000000 ) ) ;
#2633 = CARTESIAN_POINT ( 'NONE',  ( 0.000000000000000000, 0.000000000000000000, 0.000000000000000000 ) ) ;
#2634 = AXIS2_PLACEMENT_3D ( 'NONE', #13403, #467, #14394 ) ;
#2635 = ORIENTED_EDGE ( 'NONE', *, *, #8017, .T. ) ;
#2636 = CARTESIAN_POINT ( 'NONE',  ( 21.70015242457608196, -7.699555573020137267, -85.52161047917867620 ) ) ;
#2637 = CARTESIAN_POINT ( 'NONE',  ( 3.600000000000060485, 10.82531754730546147, 46.00000000000000711 ) ) ;
#2638 = CARTESIAN_POINT ( 'NONE',  ( 16.62983158603121936, 6.888301780572501976, -7.460112499819690157 ) ) ;
#2639 = CIRCLE ( 'NONE', #8049, 2.649999999999987477 ) ;
#2640 = VERTEX_POINT ( 'NONE', #19819 ) ;
#2641 = ORIENTED_EDGE ( 'NONE', *, *, #11407, .T. ) ;
#2642 = CARTESIAN_POINT ( 'NONE',  ( 19.99999999999999645, -64.79224928664389438, -2.456263514198281150 ) ) ;
#2643 = VECTOR ( 'NONE', #19368, 1000.000000000000000 ) ;
#2644 = DIRECTION ( 'NONE',  ( -1.000000000000000000, -0.000000000000000000, 0.000000000000000000 ) ) ;
#2645 = CARTESIAN_POINT ( 'NONE',  ( -52.49999999999999289, -40.00000000000000000, 5.000000000000000000 ) ) ;
#2646 = DIRECTION ( 'NONE',  ( -1.000000000000000000, -0.000000000000000000, 0.000000000000000000 ) ) ;
#2647 = EDGE_CURVE ( 'NONE', #11011, #10416, #20768, .T. ) ;
#2648 = CARTESIAN_POINT ( 'NONE',  ( 15.25966316918061771, -10.19618095414378800, 5.342143750180310846 ) ) ;
#2649 = EDGE_CURVE ( 'NONE', #19553, #19211, #5300, .T. ) ;
#2650 = CARTESIAN_POINT ( 'NONE',  ( -2.870125741905213079, 6.929096494179683319, -15.15661249981968517 ) ) ;
#2651 = ORIENTED_EDGE ( 'NONE', *, *, #399, .F. ) ;
#2652 = DIRECTION ( 'NONE',  ( 0.000000000000000000, 0.000000000000000000, 1.000000000000000000 ) ) ;
#2653 = CARTESIAN_POINT ( 'NONE',  ( -14.79893867758296544, 1.779018419858780125E-09, 14.83470808151907683 ) ) ;
#2654 = EDGE_CURVE ( 'NONE', #19812, #18469, #9965, .T. ) ;
#2655 = CARTESIAN_POINT ( 'NONE',  ( 150.0000507999999968, 0.000000000000000000, 0.000000000000000000 ) ) ;
#2656 = ORIENTED_EDGE ( 'NONE', *, *, #20426, .F. ) ;
#2657 = FACE_OUTER_BOUND ( 'NONE', #14793, .T. ) ;
#2658 = CARTESIAN_POINT ( 'NONE',  ( -6.888301784570738384, -16.62983158437509346, -20.87113749981968880 ) ) ;
#2659 = DIRECTION ( 'NONE',  ( 0.000000000000000000, -0.9422609221188236184, 0.3348796121709771145 ) ) ;
#2660 = ORIENTED_EDGE ( 'NONE', *, *, #20515, .F. ) ;
#2661 = DIRECTION ( 'NONE',  ( 0.000000000000000000, -0.000000000000000000, 1.000000000000000000 ) ) ;
#2662 = ORIENTED_EDGE ( 'NONE', *, *, #19573, .T. ) ;
#2663 = DIRECTION ( 'NONE',  ( -1.000000000000000000, 0.000000000000000000, 0.000000000000000000 ) ) ;
#2664 = LINE ( 'NONE', #12623, #19397 ) ;
#2665 = ORIENTED_EDGE ( 'NONE', *, *, #5993, .F. ) ;
#2666 = ORIENTED_EDGE ( 'NONE', *, *, #14193, .F. ) ;
#2667 = CARTESIAN_POINT ( 'NONE',  ( 36.51810716189519468, -119.7975043377066697, -78.43191108116040766 ) ) ;
#2668 = CARTESIAN_POINT ( 'NONE',  ( 19.99999999999999645, -36.54710069451090959, 54.05313526368099986 ) ) ;
#2669 = CARTESIAN_POINT ( 'NONE',  ( 0.000000000000000000, 64.79224928664386596, 2.456263514198732345 ) ) ;
#2670 = CARTESIAN_POINT ( 'NONE',  ( -1.491842756249031510, -7.499999999820660790, -25.25041874981968704 ) ) ;
#2671 = CYLINDRICAL_SURFACE ( 'NONE', #14285, 27.60000000002760245 ) ;
#2672 = LINE ( 'NONE', #18989, #32 ) ;
#2673 = DIRECTION ( 'NONE',  ( 0.000000000000000000, 1.000000000000000000, -8.673617379884034239E-17 ) ) ;
#2674 = ORIENTED_EDGE ( 'NONE', *, *, #1796, .T. ) ;
#2675 = CYLINDRICAL_SURFACE ( 'NONE', #9198, 8.500000000000000000 ) ;
#2676 = ORIENTED_EDGE ( 'NONE', *, *, #8532, .F. ) ;
#2677 = CARTESIAN_POINT ( 'NONE',  ( -10.19618095047498052, 15.25966317163203101, -10.11089374981968625 ) ) ;
#2678 = DIRECTION ( 'NONE',  ( -0.000000000000000000, -0.000000000000000000, -1.000000000000000000 ) ) ;
#2679 = ORIENTED_EDGE ( 'NONE', *, *, #18054, .T. ) ;
#2680 = DIRECTION ( 'NONE',  ( -1.000000000000000000, -0.000000000000000000, -0.000000000000000000 ) ) ;
#2681 = ORIENTED_EDGE ( 'NONE', *, *, #3636, .T. ) ;
#2682 = DIRECTION ( 'NONE',  ( 0.000000000000000000, 0.000000000000000000, -1.000000000000000000 ) ) ;
#2683 = FACE_OUTER_BOUND ( 'NONE', #3001, .T. ) ;
#2684 = CARTESIAN_POINT ( 'NONE',  ( 6.358192988180014993, 4.248408729364578917, -0.5097937498196938311 ) ) ;
#2685 = ADVANCED_FACE ( 'NONE', ( #16748 ), #5195, .F. ) ;
#2686 = ORIENTED_EDGE ( 'NONE', *, *, #12480, .F. ) ;
#2687 = CARTESIAN_POINT ( 'NONE',  ( -2.870125743571144028, -6.929096493489630859, -18.69098749981968410 ) ) ;
#2688 = DIRECTION ( 'NONE',  ( 0.000000000000000000, 0.000000000000000000, -1.000000000000000000 ) ) ;
#2689 = CARTESIAN_POINT ( 'NONE',  ( 17.99999999999999645, -2.163824016901520184E-09, -25.72104999981969442 ) ) ;
#2690 = CARTESIAN_POINT ( 'NONE',  ( -30.00000000000000000, -170.8299878242309546, 15.48896927112552824 ) ) ;
#2691 = CARTESIAN_POINT ( 'NONE',  ( 0.000000000000000000, 64.79224928664392280, 25.14373648582975918 ) ) ;
#2692 = VERTEX_POINT ( 'NONE', #11772 ) ;
#2693 = CARTESIAN_POINT ( 'NONE',  ( 0.000000000000000000, -64.79224928664389438, 25.14373648582931864 ) ) ;
#2694 = VERTEX_POINT ( 'NONE', #1918 ) ;
#2695 = CARTESIAN_POINT ( 'NONE',  ( 50.00000000000000000, -29.99999999999999645, -45.00000000000000000 ) ) ;
#2696 = FACE_OUTER_BOUND ( 'NONE', #6888, .T. ) ;
#2697 = VERTEX_POINT ( 'NONE', #434 ) ;
#2698 = CARTESIAN_POINT ( 'NONE',  ( 3.580422610670020322, -18.00000000043041126, -12.32973124981968560 ) ) ;
#2699 = FACE_OUTER_BOUND ( 'NONE', #9816, .T. ) ;
#2700 = DIRECTION ( 'NONE',  ( 0.000000000000000000, 0.8169698930104432044, -0.5766803221148655290 ) ) ;
#2701 = VERTEX_POINT ( 'NONE', #13476 ) ;
#2702 = DIRECTION ( 'NONE',  ( -1.000000000000000000, 0.000000000000000000, 0.000000000000000000 ) ) ;
#2703 = ORIENTED_EDGE ( 'NONE', *, *, #3092, .F. ) ;
#2704 = CARTESIAN_POINT ( 'NONE',  ( 50.00000000000000000, -164.9999999999999716, -90.00000000000001421 ) ) ;
#2705 = EDGE_CURVE ( 'NONE', #4710, #10182, #10175, .T. ) ;
#2706 = ORIENTED_EDGE ( 'NONE', *, *, #18009, .T. ) ;
#2707 = FACE_OUTER_BOUND ( 'NONE', #6289, .T. ) ;
#2708 = ADVANCED_FACE ( 'NONE', ( #10393 ), #8688, .T. ) ;
#2709 = CARTESIAN_POINT ( 'NONE',  ( -49.35000000000000142, -99.99999999999998579, 0.000000000000000000 ) ) ;
#2710 = CARTESIAN_POINT ( 'NONE',  ( 13.67243654642775574, -5.663308650141541278, -2.520645581158456938 ) ) ;
#2711 = ORIENTED_EDGE ( 'NONE', *, *, #13485, .T. ) ;
#2712 = DIRECTION ( 'NONE',  ( 0.000000000000000000, 0.000000000000000000, -1.000000000000000000 ) ) ;
#2713 = ORIENTED_EDGE ( 'NONE', *, *, #2855, .T. ) ;
#2714 = CARTESIAN_POINT ( 'NONE',  ( 2.870125741905212635, -6.929096494179677101, -26.13401249981969343 ) ) ;
#2715 = CARTESIAN_POINT ( 'NONE',  ( 12.72792206288790773, 12.72792205982779912, 1.375825000180311175 ) ) ;
#2716 = CARTESIAN_POINT ( 'NONE',  ( 0.000000000000000000, 0.000000000000000000, 0.000000000000000000 ) ) ;
#2717 = CIRCLE ( 'NONE', #4068, 8.999999999999998224 ) ;
#2718 = DIRECTION ( 'NONE',  ( 0.000000000000000000, -0.5000000000000011102, -0.8660254037844379305 ) ) ;
#2719 = ORIENTED_EDGE ( 'NONE', *, *, #6257, .T. ) ;
#2720 = FACE_OUTER_BOUND ( 'NONE', #10015, .T. ) ;
#2721 = DIRECTION ( 'NONE',  ( -0.000000000000000000, -0.000000000000000000, 1.000000000000000000 ) ) ;
#2722 = AXIS2_PLACEMENT_3D ( 'NONE', #7827, #7939, #18669 ) ;
#2723 = ORIENTED_EDGE ( 'NONE', *, *, #4912, .F. ) ;
#2724 = CARTESIAN_POINT ( 'NONE',  ( -3.019303355814636269, -22.81398296884255927, -75.45291102792386084 ) ) ;
#2725 = DIRECTION ( 'NONE',  ( -0.6156453966108041964, 0.000000000000000000, 0.7880233154113687188 ) ) ;
#2726 = CARTESIAN_POINT ( 'NONE',  ( 15.25966317163202568, 10.19618095047498230, -17.17964374981969300 ) ) ;
#2727 = ORIENTED_EDGE ( 'NONE', *, *, #20108, .F. ) ;
#2728 = DIRECTION ( 'NONE',  ( 0.000000000000000000, 0.000000000000000000, 1.000000000000000000 ) ) ;
#2729 = ADVANCED_FACE ( 'NONE', ( #14850 ), #640, .T. ) ;
#2730 = CARTESIAN_POINT ( 'NONE',  ( 30.00000000000000000, -99.99999999999998579, -52.00000000000000000 ) ) ;
#2731 = EDGE_CURVE ( 'NONE', #7766, #14029, #20375, .T. ) ;
#2732 = AXIS2_PLACEMENT_3D ( 'NONE', #17567, #3034, #9494 ) ;
#2733 = LINE ( 'NONE', #15662, #16649 ) ;
#2734 = CARTESIAN_POINT ( 'NONE',  ( 0.000000000000000000, -42.42902769288568976, 49.02903636734183124 ) ) ;
#2735 = CARTESIAN_POINT ( 'NONE',  ( 39.99999999999964473, -99.99999999999943157, 52.00000000000135003 ) ) ;
#2736 = CARTESIAN_POINT ( 'NONE',  ( 12.72792205982779912, -12.72792206288791483, 5.636675000180307649 ) ) ;
#2737 = AXIS2_PLACEMENT_3D ( 'NONE', #16873, #20253, #19933 ) ;
#2738 = EDGE_CURVE ( 'NONE', #15842, #6855, #3781, .T. ) ;
#2739 = EDGE_CURVE ( 'NONE', #13850, #1999, #15979, .T. ) ;
#2740 = DIRECTION ( 'NONE',  ( 0.000000000000000000, 0.000000000000000000, 1.000000000000000000 ) ) ;
#2741 = VECTOR ( 'NONE', #14956, 1000.000000000000000 ) ;
#2742 = EDGE_CURVE ( 'NONE', #10180, #19485, #19690, .T. ) ;
#2743 = ORIENTED_EDGE ( 'NONE', *, *, #6389, .T. ) ;
#2744 = CARTESIAN_POINT ( 'NONE',  ( 19.99999999999999645, -58.44960523466261293, 28.06621538408569805 ) ) ;
#2745 = CARTESIAN_POINT ( 'NONE',  ( 10.32494394706615637, -4.276731815070946574, -27.74104725028680463 ) ) ;
#2746 = FACE_OUTER_BOUND ( 'NONE', #9484, .T. ) ;
#2747 = VERTEX_POINT ( 'NONE', #5711 ) ;
#2748 = CARTESIAN_POINT ( 'NONE',  ( 1.321505333908968627, -3.855830693249186147, -0.03421028094655685636 ) ) ;
#2749 = CARTESIAN_POINT ( 'NONE',  ( 16.62983158603122291, 6.888301780572502864, -14.98051249981969058 ) ) ;
#2750 = DIRECTION ( 'NONE',  ( -1.000000000000000000, 0.000000000000000000, 0.000000000000000000 ) ) ;
#2751 = VERTEX_POINT ( 'NONE', #6039 ) ;
#2752 = EDGE_CURVE ( 'NONE', #12799, #9697, #10910, .T. ) ;
#2753 = DIRECTION ( 'NONE',  ( 1.000000000000000000, -0.000000000000000000, -0.000000000000000000 ) ) ;
#2754 = AXIS2_PLACEMENT_3D ( 'NONE', #1842, #4914, #17858 ) ;
#2755 = ORIENTED_EDGE ( 'NONE', *, *, #6976, .T. ) ;
#2756 = DIRECTION ( 'NONE',  ( 0.000000000000000000, 0.7308359642781253607, -0.6825531432186527914 ) ) ;
#2757 = CARTESIAN_POINT ( 'NONE',  ( -6.359999999999999432, 10.85999999999999943, 0.000000000000000000 ) ) ;
#2758 = ORIENTED_EDGE ( 'NONE', *, *, #280, .T. ) ;
#2759 = AXIS2_PLACEMENT_3D ( 'NONE', #11981, #13478, #7196 ) ;
#2760 = ORIENTED_EDGE ( 'NONE', *, *, #2440, .T. ) ;
#2761 = CARTESIAN_POINT ( 'NONE',  ( 37.15969169416875673, -120.3577465631687033, -78.81653076392491641 ) ) ;
#2762 = ADVANCED_FACE ( 'NONE', ( #1183 ), #20654, .F. ) ;
#2763 = CIRCLE ( 'NONE', #4454, 2.650000000000000355 ) ;
#2764 = DIRECTION ( 'NONE',  ( -0.5000000000000051070, 1.060575238724903217E-16, -0.8660254037844355990 ) ) ;
#2765 = EDGE_CURVE ( 'NONE', #8003, #8586, #13958, .T. ) ;
#2766 = DIRECTION ( 'NONE',  ( 1.000000000000000000, 0.000000000000000000, -0.000000000000000000 ) ) ;
#2767 = AXIS2_PLACEMENT_3D ( 'NONE', #12595, #19062, #7495 ) ;
#2768 = AXIS2_PLACEMENT_3D ( 'NONE', #15496, #987, #18787 ) ;
#2769 = CARTESIAN_POINT ( 'NONE',  ( 7.500000000000000888, -9.015933403756337545E-10, -18.47619999981969130 ) ) ;
#2770 = AXIS2_PLACEMENT_3D ( 'NONE', #20102, #2409, #8869 ) ;
#2771 = CARTESIAN_POINT ( 'NONE',  ( 6.249999999999902300, -10.82531754730554496, 169.0000000000000000 ) ) ;
#2772 = DIRECTION ( 'NONE',  ( -1.000000000000000000, -0.000000000000000000, -0.000000000000000000 ) ) ;
#2773 = ORIENTED_EDGE ( 'NONE', *, *, #15336, .T. ) ;
#2774 = CARTESIAN_POINT ( 'NONE',  ( 2.500000000000000000, 2.357898499370431722, -2.818925648462311528E-15 ) ) ;
#2775 = VERTEX_POINT ( 'NONE', #2860 ) ;
#2776 = CARTESIAN_POINT ( 'NONE',  ( 3.580422614997668340, 17.99999999956958519, -8.932768749819690157 ) ) ;
#2777 = DIRECTION ( 'NONE',  ( -1.000000000000000000, 0.000000000000000000, -0.000000000000000000 ) ) ;
#2778 = VECTOR ( 'NONE', #15661, 1000.000000000000000 ) ;
#2779 = ORIENTED_EDGE ( 'NONE', *, *, #6739, .T. ) ;
#2780 = EDGE_CURVE ( 'NONE', #15314, #3307, #15642, .T. ) ;
#2781 = DIRECTION ( 'NONE',  ( 1.000000000000000000, 0.000000000000000000, 0.000000000000000000 ) ) ;
#2782 = VERTEX_POINT ( 'NONE', #9325 ) ;
#2783 = CARTESIAN_POINT ( 'NONE',  ( 4.248408729364576253, -6.358192988180015881, -7.578543749819692366 ) ) ;
#2784 = CARTESIAN_POINT ( 'NONE',  ( 50.00000000000000000, -164.9999999999999716, 75.59990929030060158 ) ) ;
#2785 = CYLINDRICAL_SURFACE ( 'NONE', #6653, 80.00000000000000000 ) ;
#2786 = EDGE_LOOP ( 'NONE', ( #4513, #3181 ) ) ;
#2787 = CARTESIAN_POINT ( 'NONE',  ( 19.99999999999999645, -63.17103598352115057, -16.33561182745204476 ) ) ;
#2788 = AXIS2_PLACEMENT_3D ( 'NONE', #13993, #20450, #5930 ) ;
#2789 = AXIS2_PLACEMENT_3D ( 'NONE', #20333, #4238, #12405 ) ;
#2790 = CARTESIAN_POINT ( 'NONE',  ( 24.99999999999999645, -39.99999999999999289, -52.00000000000000000 ) ) ;
#2791 = DIRECTION ( 'NONE',  ( -1.000000000000000000, 0.000000000000000000, 0.000000000000000000 ) ) ;
#2792 = LINE ( 'NONE', #17536, #14704 ) ;
#2793 = CARTESIAN_POINT ( 'NONE',  ( 17.50000000000000355, 2.143131898507868643E-15, 46.00000000000000711 ) ) ;
#2794 = ORIENTED_EDGE ( 'NONE', *, *, #8821, .T. ) ;
#2795 = CARTESIAN_POINT ( 'NONE',  ( 19.99999999999999645, 11.98658579560587789, 64.13855129306472236 ) ) ;
#2796 = ADVANCED_FACE ( 'NONE', ( #10606 ), #8898, .T. ) ;
#2797 = DIRECTION ( 'NONE',  ( -1.000000000000000000, -0.000000000000000000, 0.000000000000000000 ) ) ;
#2798 = ORIENTED_EDGE ( 'NONE', *, *, #14879, .T. ) ;
#2799 = VECTOR ( 'NONE', #19885, 1000.000000000000000 ) ;
#2800 = CARTESIAN_POINT ( 'NONE',  ( 19.99999999999999645, 65.23577793412344761, -1.313498510941930153 ) ) ;
#2801 = LINE ( 'NONE', #6291, #11609 ) ;
#2802 = CIRCLE ( 'NONE', #2461, 2.649999999999987477 ) ;
#2803 = ORIENTED_EDGE ( 'NONE', *, *, #8889, .T. ) ;
#2804 = CARTESIAN_POINT ( 'NONE',  ( 10.19618095047497874, -15.25966317163203279, -22.34379374981968880 ) ) ;
#2805 = VECTOR ( 'NONE', #6216, 1000.000000000000000 ) ;
#2806 = DIRECTION ( 'NONE',  ( -0.000000000000000000, -0.000000000000000000, 1.000000000000000000 ) ) ;
#2807 = DIRECTION ( 'NONE',  ( 0.000000000000000000, 0.000000000000000000, 1.000000000000000000 ) ) ;
#2808 = EDGE_LOOP ( 'NONE', ( #2337, #15718, #1779, #1264 ) ) ;
#2809 = DIRECTION ( 'NONE',  ( -1.000000000000000000, 0.000000000000000000, 0.000000000000000000 ) ) ;
#2810 = ORIENTED_EDGE ( 'NONE', *, *, #5239, .F. ) ;
#2811 = DIRECTION ( 'NONE',  ( -1.000000000000000000, -0.000000000000000000, -0.000000000000000000 ) ) ;
#2812 = ORIENTED_EDGE ( 'NONE', *, *, #7995, .F. ) ;
#2813 = FACE_OUTER_BOUND ( 'NONE', #1797, .T. ) ;
#2814 = AXIS2_PLACEMENT_3D ( 'NONE', #14812, #918, #10556 ) ;
#2815 = AXIS2_PLACEMENT_3D ( 'NONE', #1548, #5112, #17955 ) ;
#2816 = CYLINDRICAL_SURFACE ( 'NONE', #2827, 27.60000000002760245 ) ;
#2817 = CARTESIAN_POINT ( 'NONE',  ( 10.46442989202484064, -10.46442989454075878, 7.493416918841544927 ) ) ;
#2818 = VERTEX_POINT ( 'NONE', #17280 ) ;
#2819 = EDGE_CURVE ( 'NONE', #2406, #9297, #17068, .T. ) ;
#2820 = CARTESIAN_POINT ( 'NONE',  ( -4.000000000000000000, -1.549102112939103826, -5.442104661404060906 ) ) ;
#2821 = ORIENTED_EDGE ( 'NONE', *, *, #4143, .F. ) ;
#2822 = CIRCLE ( 'NONE', #3156, 17.50000000000000355 ) ;
#2823 = CARTESIAN_POINT ( 'NONE',  ( -1.464933908330800394, -21.46223383259977879, 76.05833375614351155 ) ) ;
#2824 = CARTESIAN_POINT ( 'NONE',  ( 17.99999999999999645, -2.163824016901520184E-09, 11.97895000018031020 ) ) ;
#2825 = CARTESIAN_POINT ( 'NONE',  ( -17.50000000000000355, 0.000000000000000000, -43.00000000000000000 ) ) ;
#2826 = CARTESIAN_POINT ( 'NONE',  ( 2.500000000000000000, -1.178949249685213863, 2.042000000000002924 ) ) ;
#2827 = AXIS2_PLACEMENT_3D ( 'NONE', #6406, #1448, #4618 ) ;
#2828 = AXIS2_PLACEMENT_3D ( 'NONE', #3495, #1412, #7862 ) ;
#2829 = VERTEX_POINT ( 'NONE', #7627 ) ;
#2830 = DIRECTION ( 'NONE',  ( -1.000000000000000000, 0.000000000000000000, 0.000000000000000000 ) ) ;
#2831 = FACE_BOUND ( 'NONE', #9265, .T. ) ;
#2832 = ORIENTED_EDGE ( 'NONE', *, *, #3897, .F. ) ;
#2833 = CARTESIAN_POINT ( 'NONE',  ( 19.24126430796853171, -12.61765026593414873, -81.34437286535597877 ) ) ;
#2834 = FACE_OUTER_BOUND ( 'NONE', #14790, .T. ) ;
#2835 = CARTESIAN_POINT ( 'NONE',  ( -3.580422610670017658, 18.00000000043040771, -18.94683124981969158 ) ) ;
#2836 = AXIS2_PLACEMENT_3D ( 'NONE', #11379, #9882, #17856 ) ;
#2837 = ORIENTED_EDGE ( 'NONE', *, *, #2262, .T. ) ;
#2838 = CARTESIAN_POINT ( 'NONE',  ( -7.500000000000009770, 9.706494115329868228E-15, -7.498799999997683763 ) ) ;
#2839 = CIRCLE ( 'NONE', #1830, 27.60000000002759535 ) ;
#2840 = CARTESIAN_POINT ( 'NONE',  ( 9.999999999999998224, 18.50424539729845463, 69.58155576219121485 ) ) ;
#2841 = FACE_BOUND ( 'NONE', #19630, .T. ) ;
#2842 = CARTESIAN_POINT ( 'NONE',  ( 0.000000000000000000, 0.9548212943365497196, 71.99366858485716136 ) ) ;
#2843 = CARTESIAN_POINT ( 'NONE',  ( 6.249999999999902300, -10.82531754730554496, -51.00000000000001421 ) ) ;
#2844 = CARTESIAN_POINT ( 'NONE',  ( -17.99999999956958874, 3.580422614997675002, 0.04058125018030836473 ) ) ;
#2845 = AXIS2_PLACEMENT_3D ( 'NONE', #17316, #15610, #20491 ) ;
#2846 = AXIS2_PLACEMENT_3D ( 'NONE', #18057, #19325, #16558 ) ;
#2847 = CARTESIAN_POINT ( 'NONE',  ( 7.499999999820668783, -1.491842756249033508, -21.34176874981968908 ) ) ;
#2848 = ORIENTED_EDGE ( 'NONE', *, *, #15763, .F. ) ;
#2849 = PLANE ( 'NONE',  #18202 ) ;
#2850 = CARTESIAN_POINT ( 'NONE',  ( 5.663308650141530620, 13.67243654642775041, 8.355020581519076117 ) ) ;
#2851 = CIRCLE ( 'NONE', #3523, 2.099999999999999645 ) ;
#2852 = EDGE_CURVE ( 'NONE', #11740, #5793, #1443, .T. ) ;
#2853 = ORIENTED_EDGE ( 'NONE', *, *, #6566, .F. ) ;
#2854 = DIRECTION ( 'NONE',  ( 0.000000000000000000, 0.000000000000000000, 1.000000000000000000 ) ) ;
#2855 = EDGE_CURVE ( 'NONE', #19557, #3608, #7853, .T. ) ;
#2856 = CARTESIAN_POINT ( 'NONE',  ( -12.72792205982779912, 12.72792206288790950, -17.92582499981968880 ) ) ;
#2857 = LINE ( 'NONE', #13886, #920 ) ;
#2858 = AXIS2_PLACEMENT_3D ( 'NONE', #2035, #4910, #12874 ) ;
#2859 = ORIENTED_EDGE ( 'NONE', *, *, #20832, .F. ) ;
#2860 = CARTESIAN_POINT ( 'NONE',  ( 19.99999999999999645, 56.42118728228200553, -32.77318456705383198 ) ) ;
#2861 = ORIENTED_EDGE ( 'NONE', *, *, #16747, .T. ) ;
#2862 = CIRCLE ( 'NONE', #14712, 0.3200000000000017275 ) ;
#2863 = CARTESIAN_POINT ( 'NONE',  ( 19.99999999999999645, 56.63599015375715595, -31.56633360682406675 ) ) ;
#2864 = DIRECTION ( 'NONE',  ( 0.000000000000000000, 0.000000000000000000, 1.000000000000000000 ) ) ;
#2865 = ORIENTED_EDGE ( 'NONE', *, *, #2103, .T. ) ;
#2866 = EDGE_CURVE ( 'NONE', #8899, #14496, #2102, .T. ) ;
#2867 = ORIENTED_EDGE ( 'NONE', *, *, #10506, .F. ) ;
#2868 = DIRECTION ( 'NONE',  ( -0.000000000000000000, -0.000000000000000000, 1.000000000000000000 ) ) ;
#2869 = FACE_OUTER_BOUND ( 'NONE', #5666, .T. ) ;
#2870 = DIRECTION ( 'NONE',  ( 1.000000000000000000, 0.000000000000000000, 0.000000000000000000 ) ) ;
#2871 = CARTESIAN_POINT ( 'NONE',  ( 7.902369978624329327, 7.902369976724401113, -12.96051524935257682 ) ) ;
#2872 = EDGE_CURVE ( 'NONE', #19105, #18360, #10226, .T. ) ;
#2873 = PRESENTATION_LAYER_ASSIGNMENT (  '', '', ( #162 ) ) ;
#2874 = CARTESIAN_POINT ( 'NONE',  ( -6.330490858644137298, -9.474249097082495297, 12.60973399971320141 ) ) ;
#2875 = FACE_OUTER_BOUND ( 'NONE', #7065, .T. ) ;
#2876 = FACE_OUTER_BOUND ( 'NONE', #7626, .T. ) ;
#2877 = CARTESIAN_POINT ( 'NONE',  ( 30.00000000000000000, -50.00000000000000000, -90.00000000000001421 ) ) ;
#2878 = ADVANCED_FACE ( 'NONE', ( #13789 ), #20240, .T. ) ;
#2879 = ORIENTED_EDGE ( 'NONE', *, *, #9976, .T. ) ;
#2880 = PLANE ( 'NONE',  #15289 ) ;
#2881 = ADVANCED_FACE ( 'NONE', ( #7514 ), #78, .F. ) ;
#2882 = ORIENTED_EDGE ( 'NONE', *, *, #1261, .T. ) ;
#2883 = CARTESIAN_POINT ( 'NONE',  ( -3.580422610670018546, 18.00000000043041126, -9.521831249819687315 ) ) ;
#2884 = DIRECTION ( 'NONE',  ( 0.000000000000000000, 0.7308359642781253607, -0.6825531432186527914 ) ) ;
#2885 = EDGE_LOOP ( 'NONE', ( #3168, #14036, #4906, #619 ) ) ;
#2886 = ORIENTED_EDGE ( 'NONE', *, *, #6253, .T. ) ;
#2887 = DIRECTION ( 'NONE',  ( -1.000000000000000000, -0.000000000000000000, -0.000000000000000000 ) ) ;
#2888 = EDGE_LOOP ( 'NONE', ( #11612, #13345, #13289, #12087, #993, #4415, #17877, #15738, #10933, #2798, #11922, #17154, #17493, #858, #7916, #13524, #16055, #8102, #14543, #11910, #12792, #19990, #12548, #8448, #1874, #18556, #2338, #1405 ) ) ;
#2889 = DIRECTION ( 'NONE',  ( 1.000000000000000000, 0.000000000000000000, 0.000000000000000000 ) ) ;
#2890 = DIRECTION ( 'NONE',  ( 1.000000000000000000, 0.000000000000000000, -0.000000000000000000 ) ) ;
#2891 = CARTESIAN_POINT ( 'NONE',  ( 0.000000000000000000, 0.000000000000000000, -84.99999999999998579 ) ) ;
#2892 = EDGE_CURVE ( 'NONE', #8586, #964, #11913, .T. ) ;
#2893 = ORIENTED_EDGE ( 'NONE', *, *, #5507, .F. ) ;
#2894 = CARTESIAN_POINT ( 'NONE',  ( 30.00000000000000711, -30.00000000000001421, -120.0000000000000142 ) ) ;
#2895 = CIRCLE ( 'NONE', #4920, 72.00000000007199219 ) ;
#2896 = CARTESIAN_POINT ( 'NONE',  ( 3.599999999999909051, -10.82531754730554496, 166.0000000000000000 ) ) ;
#2897 = CARTESIAN_POINT ( 'NONE',  ( -6.888301780572500199, 16.62983158603121936, -19.24136249981969016 ) ) ;
#2898 = CYLINDRICAL_SURFACE ( 'NONE', #12686, 10.52399999999999558 ) ;
#2899 = CARTESIAN_POINT ( 'NONE',  ( 6.250000000000054179, 10.82531754730546147, 43.00000000000000000 ) ) ;
#2900 = ORIENTED_EDGE ( 'NONE', *, *, #12503, .T. ) ;
#2901 = ADVANCED_FACE ( 'NONE', ( #10715 ), #17179, .F. ) ;
#2902 = EDGE_CURVE ( 'NONE', #19080, #14722, #9435, .T. ) ;
#2903 = CARTESIAN_POINT ( 'NONE',  ( 0.000000000000000000, -56.63599015375651646, -31.56633360682521072 ) ) ;
#2904 = CIRCLE ( 'NONE', #14750, 27.60000000002759535 ) ;
#2905 = DIRECTION ( 'NONE',  ( -1.000000000000000000, -0.000000000000000000, 0.000000000000000000 ) ) ;
#2906 = ORIENTED_EDGE ( 'NONE', *, *, #11299, .T. ) ;
#2907 = DIRECTION ( 'NONE',  ( 0.000000000000000000, 0.8169698930104430934, -0.5766803221148655290 ) ) ;
#2908 = DIRECTION ( 'NONE',  ( -1.000000000000000000, -0.000000000000000000, 0.000000000000000000 ) ) ;
#2909 = VECTOR ( 'NONE', #8162, 1000.000000000000000 ) ;
#2910 = VERTEX_POINT ( 'NONE', #14723 ) ;
#2911 = CARTESIAN_POINT ( 'NONE',  ( -10.19618095414378622, -15.25966316918061416, -11.15160624981969129 ) ) ;
#2912 = EDGE_CURVE ( 'NONE', #714, #5717, #3455, .T. ) ;
#2913 = DIRECTION ( 'NONE',  ( 1.000000000000000000, -0.000000000000000000, -0.000000000000000000 ) ) ;
#2914 = CARTESIAN_POINT ( 'NONE',  ( -30.00000000000000000, -30.00000000000000000, -130.0000000000000000 ) ) ;
#2915 = ORIENTED_EDGE ( 'NONE', *, *, #13097, .F. ) ;
#2916 = LINE ( 'NONE', #12462, #17712 ) ;
#2917 = ORIENTED_EDGE ( 'NONE', *, *, #14896, .F. ) ;
#2918 = DIRECTION ( 'NONE',  ( 1.000000000000000000, 1.836909530733573776E-16, 0.000000000000000000 ) ) ;
#2919 = VERTEX_POINT ( 'NONE', #1696 ) ;
#2920 = AXIS2_PLACEMENT_3D ( 'NONE', #9422, #17263, #7819 ) ;
#2921 = AXIS2_PLACEMENT_3D ( 'NONE', #8178, #14961, #14646 ) ;
#2922 = CARTESIAN_POINT ( 'NONE',  ( 0.000000000000000000, 0.000000000000000000, 46.00000000000000711 ) ) ;
#2923 = AXIS2_PLACEMENT_3D ( 'NONE', #7245, #13727, #685 ) ;
#2924 = CIRCLE ( 'NONE', #8006, 2.041999999999999815 ) ;
#2925 = CARTESIAN_POINT ( 'NONE',  ( 0.000000000000000000, 51.81019761368373366, -38.98425606966007706 ) ) ;
#2926 = ITEM_DEFINED_TRANSFORMATION ( 'NONE', 'NONE', #1869,  #12461 ) ;
#2927 = CARTESIAN_POINT ( 'NONE',  ( 2.943691928843431782, 14.79893867722910628, 4.253573168841545460 ) ) ;
#2928 = ORIENTED_EDGE ( 'NONE', *, *, #6486, .T. ) ;
#2929 = CARTESIAN_POINT ( 'NONE',  ( -6.929096494179678878, -2.870125741905209971, -14.35276249981969343 ) ) ;
#2930 = DIRECTION ( 'NONE',  ( -1.000000000000000000, -0.000000000000000000, -0.000000000000000000 ) ) ;
#2931 = ORIENTED_EDGE ( 'NONE', *, *, #2738, .T. ) ;
#2932 = DIRECTION ( 'NONE',  ( 1.000000000000000000, 0.000000000000000000, 0.000000000000000000 ) ) ;
#2933 = CIRCLE ( 'NONE', #4625, 10.85999999999999410 ) ;
#2934 = VECTOR ( 'NONE', #5279, 1000.000000000000000 ) ;
#2935 = CARTESIAN_POINT ( 'NONE',  ( -6.358192987158592047, 4.248408730893246776, -22.30510624981969414 ) ) ;
#2936 = CARTESIAN_POINT ( 'NONE',  ( -32.96694501150314949, -24.74873734152930993, -130.0000000000000000 ) ) ;
#2937 = AXIS2_PLACEMENT_3D ( 'NONE', #14418, #16204, #6349 ) ;
#2938 = AXIS2_PLACEMENT_3D ( 'NONE', #594, #4180, #18602 ) ;
#2939 = ORIENTED_EDGE ( 'NONE', *, *, #15465, .T. ) ;
#2940 =( GEOMETRIC_REPRESENTATION_CONTEXT ( 3 ) GLOBAL_UNCERTAINTY_ASSIGNED_CONTEXT ( ( #14939 ) ) GLOBAL_UNIT_ASSIGNED_CONTEXT ( ( #5009, #5206, #15169 ) ) REPRESENTATION_CONTEXT ( 'NONE', 'WORKASPACE' ) );
#2941 = DIRECTION ( 'NONE',  ( 1.000000000000000000, 0.000000000000000000, 0.000000000000000000 ) ) ;
#2942 = LINE ( 'NONE', #12584, #19881 ) ;
#2943 = ORIENTED_EDGE ( 'NONE', *, *, #20228, .T. ) ;
#2944 = CARTESIAN_POINT ( 'NONE',  ( 0.000000000000000000, 59.31169354540738681, 27.19476070466876649 ) ) ;
#2945 = EDGE_CURVE ( 'NONE', #17868, #15579, #11337, .T. ) ;
#2946 = CARTESIAN_POINT ( 'NONE',  ( 1.491842754445842578, -7.500000000179340987, 2.435518750180307723 ) ) ;
#2947 = CARTESIAN_POINT ( 'NONE',  ( -12.72792206288790950, -12.72792205982779556, -22.18667499981969726 ) ) ;
#2948 = EDGE_CURVE ( 'NONE', #15833, #13416, #11018, .T. ) ;
#2949 = ORIENTED_EDGE ( 'NONE', *, *, #12308, .F. ) ;
#2950 = CARTESIAN_POINT ( 'NONE',  ( -9.015947181032835626E-10, -7.500000000000007994, -9.855049999819689432 ) ) ;
#2951 = FACE_OUTER_BOUND ( 'NONE', #19937, .T. ) ;
#2952 = AXIS2_PLACEMENT_3D ( 'NONE', #14706, #6633, #13118 ) ;
#2953 = DIRECTION ( 'NONE',  ( 0.000000000000000000, 0.000000000000000000, -1.000000000000000000 ) ) ;
#2954 = DIRECTION ( 'NONE',  ( -1.384478184788908018E-16, 1.611744734445712550E-26, 1.000000000000000000 ) ) ;
#2955 = CARTESIAN_POINT ( 'NONE',  ( -36.99999999999999289, -85.00000000000000000, -1.040949779275250179E-14 ) ) ;
#2956 = CARTESIAN_POINT ( 'NONE',  ( -17.99999999956958874, 3.580422614997675002, 9.465581250180308714 ) ) ;
#2957 = CIRCLE ( 'NONE', #1932, 10.00000000000000178 ) ;
#2958 = CARTESIAN_POINT ( 'NONE',  ( 6.929096494179683319, 2.870125741905213079, -12.80036249981968766 ) ) ;
#2959 = ORIENTED_EDGE ( 'NONE', *, *, #16591, .F. ) ;
#2960 = DIRECTION ( 'NONE',  ( -1.000000000000000000, 0.000000000000000000, 0.000000000000000000 ) ) ;
#2961 = CARTESIAN_POINT ( 'NONE',  ( 2.943691925285397470, -14.79893867793683349, 12.18392683151907718 ) ) ;
#2962 = DIRECTION ( 'NONE',  ( 0.000000000000000000, 0.000000000000000000, -1.000000000000000000 ) ) ;
#2963 = VECTOR ( 'NONE', #1263, 1000.000000000000000 ) ;
#2964 = EDGE_CURVE ( 'NONE', #2973, #2187, #7175, .T. ) ;
#2965 = VERTEX_POINT ( 'NONE', #3277 ) ;
#2966 = CARTESIAN_POINT ( 'NONE',  ( -24.99999999999999289, -85.00000000000000000, -9.000000000000005329 ) ) ;
#2967 = AXIS2_PLACEMENT_3D ( 'NONE', #19335, #3335, #14678 ) ;
#2968 = DIRECTION ( 'NONE',  ( 0.000000000000000000, 0.000000000000000000, -1.000000000000000000 ) ) ;
#2969 = DIRECTION ( 'NONE',  ( -1.000000000000000000, 0.000000000000000000, 0.000000000000000000 ) ) ;
#2970 = VERTEX_POINT ( 'NONE', #6550 ) ;
#2971 = FACE_BOUND ( 'NONE', #19410, .T. ) ;
#2972 = CIRCLE ( 'NONE', #10074, 72.00000000007199219 ) ;
#2973 = VERTEX_POINT ( 'NONE', #3370 ) ;
#2974 = CARTESIAN_POINT ( 'NONE',  ( 6.249999999999902300, -10.82531754730554496, 129.0000000000000000 ) ) ;
#2975 = CARTESIAN_POINT ( 'NONE',  ( 9.999999999999998224, -8.857208570070309150, 71.45313048675083678 ) ) ;
#2976 = EDGE_CURVE ( 'NONE', #15515, #659, #16108, .T. ) ;
#2977 = ORIENTED_EDGE ( 'NONE', *, *, #5731, .F. ) ;
#2978 = ORIENTED_EDGE ( 'NONE', *, *, #3510, .T. ) ;
#2979 = LINE ( 'NONE', #15689, #11376 ) ;
#2980 = CARTESIAN_POINT ( 'NONE',  ( 0.000000000000000000, 0.000000000000000000, 0.000000000000000000 ) ) ;
#2981 = EDGE_CURVE ( 'NONE', #18447, #20602, #14617, .T. ) ;
#2982 = CARTESIAN_POINT ( 'NONE',  ( 0.000000000000000000, 0.000000000000000000, 0.000000000000000000 ) ) ;
#2983 = CARTESIAN_POINT ( 'NONE',  ( 1.343451552857795926E-09, 11.17563879731705789, -14.13864024935257291 ) ) ;
#2984 = CARTESIAN_POINT ( 'NONE',  ( -1.491842754445841246, 7.500000000179339210, -21.12698124981968917 ) ) ;
#2985 = DIRECTION ( 'NONE',  ( 1.000000000000000000, 0.000000000000000000, 0.000000000000000000 ) ) ;
#2986 = ADVANCED_FACE ( 'NONE', ( #19486, #2971 ), #15891, .F. ) ;
#2987 = CARTESIAN_POINT ( 'NONE',  ( 2.500000000000002220, 3.061616997868386099E-16, -5.574599999999999334 ) ) ;
#2988 = CARTESIAN_POINT ( 'NONE',  ( -54.64999999999999858, -39.99999999999999289, 0.000000000000000000 ) ) ;
#2989 = EDGE_CURVE ( 'NONE', #18776, #16343, #9546, .T. ) ;
#2990 = ORIENTED_EDGE ( 'NONE', *, *, #16574, .F. ) ;
#2991 = CARTESIAN_POINT ( 'NONE',  ( 0.000000000000000000, 64.44931368725519860, 10.18420179740629727 ) ) ;
#2992 = ORIENTED_EDGE ( 'NONE', *, *, #14380, .T. ) ;
#2993 = CARTESIAN_POINT ( 'NONE',  ( 16.62983158603122291, 6.888301780572502864, -7.460112499819686604 ) ) ;
#2994 = CARTESIAN_POINT ( 'NONE',  ( 19.54001732319277096, -8.991134644608434812, 77.82005195698279465 ) ) ;
#2995 = ORIENTED_EDGE ( 'NONE', *, *, #17866, .T. ) ;
#2996 = CARTESIAN_POINT ( 'NONE',  ( 45.22159793441012710, -8.673994507468391291, -90.00000000000001421 ) ) ;
#2997 = EDGE_LOOP ( 'NONE', ( #1593, #20208 ) ) ;
#2998 = CARTESIAN_POINT ( 'NONE',  ( 7.500000000000004441, -8.788009017158368372E-15, -9.051199999997692203 ) ) ;
#2999 = CARTESIAN_POINT ( 'NONE',  ( -62.49999999999999289, -130.0000000000000000, 5.000000000000000000 ) ) ;
#3000 = CARTESIAN_POINT ( 'NONE',  ( -7.500000000000000000, 0.000000000000000000, 126.0000000000000000 ) ) ;
#3001 = EDGE_LOOP ( 'NONE', ( #20430, #3753 ) ) ;
#3002 = DIRECTION ( 'NONE',  ( 0.000000000000000000, 0.000000000000000000, -1.000000000000000000 ) ) ;
#3003 = DIRECTION ( 'NONE',  ( -1.000000000000000000, 0.000000000000000000, 0.000000000000000000 ) ) ;
#3004 = DIRECTION ( 'NONE',  ( -1.000000000000000000, 0.000000000000000000, 0.000000000000000000 ) ) ;
#3005 = ADVANCED_FACE ( 'NONE', ( #9834 ), #1387, .T. ) ;
#3006 = ADVANCED_FACE ( 'NONE', ( #1792 ), #7834, .T. ) ;
#3007 = LINE ( 'NONE', #2793, #5192 ) ;
#3008 = VERTEX_POINT ( 'NONE', #19183 ) ;
#3009 = EDGE_CURVE ( 'NONE', #5467, #18936, #18006, .T. ) ;
#3010 = FACE_OUTER_BOUND ( 'NONE', #11793, .T. ) ;
#3011 = ORIENTED_EDGE ( 'NONE', *, *, #2964, .F. ) ;
#3012 = EDGE_CURVE ( 'NONE', #10368, #12982, #16987, .T. ) ;
#3013 = DIRECTION ( 'NONE',  ( 0.000000000000000000, 0.3984010898462422290, -0.9172113015054527141 ) ) ;
#3014 = PLANE ( 'NONE',  #15003 ) ;
#3015 = ORIENTED_EDGE ( 'NONE', *, *, #6009, .T. ) ;
#3016 = CARTESIAN_POINT ( 'NONE',  ( 0.000000000000000000, 0.000000000000000000, 166.0000000000000000 ) ) ;
#3017 = DIRECTION ( 'NONE',  ( 0.000000000000000000, -0.7308359642781161458, -0.6825531432186624503 ) ) ;
#3018 = CARTESIAN_POINT ( 'NONE',  ( 10.00000000000000178, -160.0000000000000000, -70.00000000000000000 ) ) ;
#3019 = B_SPLINE_CURVE_WITH_KNOTS ( 'NONE', 3,
 ( #3154, #1373, #7818, #20739 ),
 .UNSPECIFIED., .F., .F.,
 ( 4, 4 ),
 ( 0.000000000000000000, 0.005429897942433520482 ),
 .UNSPECIFIED. ) ;
#3020 = ORIENTED_EDGE ( 'NONE', *, *, #4456, .T. ) ;
#3021 = DIRECTION ( 'NONE',  ( 0.000000000000000000, 0.1361666490962400444, 0.9906859460363315328 ) ) ;
#3022 = ORIENTED_EDGE ( 'NONE', *, *, #6502, .F. ) ;
#3023 = DIRECTION ( 'NONE',  ( -1.000000000000000000, -0.000000000000000000, -0.000000000000000000 ) ) ;
#3024 = ADVANCED_FACE ( 'NONE', ( #17702 ), #20865, .F. ) ;
#3025 = ORIENTED_EDGE ( 'NONE', *, *, #14545, .T. ) ;
#3026 = EDGE_CURVE ( 'NONE', #8080, #1369, #12833, .T. ) ;
#3027 = DIRECTION ( 'NONE',  ( -1.000000000000000000, 0.000000000000000000, 0.000000000000000000 ) ) ;
#3028 = ADVANCED_FACE ( 'NONE', ( #4867 ), #17808, .T. ) ;
#3029 = CARTESIAN_POINT ( 'NONE',  ( 8.900000000000046541, 10.82531754730546147, 46.00000000000000711 ) ) ;
#3030 = CONTEXT_DEPENDENT_SHAPE_REPRESENTATION ( #17817, #3726 ) ;
#3031 = CARTESIAN_POINT ( 'NONE',  ( -9.474249098604513364, -6.330490856366295382, 20.32151600064743846 ) ) ;
#3032 = ORIENTED_EDGE ( 'NONE', *, *, #3080, .F. ) ;
#3033 = CARTESIAN_POINT ( 'NONE',  ( -62.49999999999999289, -30.00000000000000000, 5.000000000000000000 ) ) ;
#3034 = DIRECTION ( 'NONE',  ( -1.000000000000000000, 0.000000000000000000, -0.000000000000000000 ) ) ;
#3035 = ORIENTED_EDGE ( 'NONE', *, *, #1972, .F. ) ;
#3036 = SHAPE_REPRESENTATION ( 'cover', ( #12461 ), #5607 ) ;
#3037 = DIRECTION ( 'NONE',  ( -1.000000000000000000, 0.000000000000000000, -0.000000000000000000 ) ) ;
#3038 = CYLINDRICAL_SURFACE ( 'NONE', #14947, 7.500000000000000000 ) ;
#3039 = CARTESIAN_POINT ( 'NONE',  ( 19.99999999999999645, 28.84646472442533494, -58.52617768068405013 ) ) ;
#3040 = VECTOR ( 'NONE', #3239, 1000.000000000000000 ) ;
#3041 = ORIENTED_EDGE ( 'NONE', *, *, #20155, .T. ) ;
#3042 = FACE_BOUND ( 'NONE', #2469, .T. ) ;
#3043 = DIRECTION ( 'NONE',  ( -0.000000000000000000, -1.000000000000000000, -0.000000000000000000 ) ) ;
#3044 =( REPRESENTATION_RELATIONSHIP ('NONE','NONE', #13739, #13064 ) REPRESENTATION_RELATIONSHIP_WITH_TRANSFORMATION ( #15430 )SHAPE_REPRESENTATION_RELATIONSHIP( ) );
#3045 = ORIENTED_EDGE ( 'NONE', *, *, #8074, .T. ) ;
#3046 = LINE ( 'NONE', #7810, #2805 ) ;
#3047 = LINE ( 'NONE', #1472, #1224 ) ;
#3048 = CARTESIAN_POINT ( 'NONE',  ( 0.000000000000000000, 0.000000000000000000, 46.00000000000000711 ) ) ;
#3049 = EDGE_LOOP ( 'NONE', ( #15005, #17734, #2074, #19128, #14741 ) ) ;
#3050 = DIRECTION ( 'NONE',  ( -0.000000000000000000, -0.000000000000000000, 1.000000000000000000 ) ) ;
#3051 = DIRECTION ( 'NONE',  ( 0.000000000000000000, 0.000000000000000000, -1.000000000000000000 ) ) ;
#3052 = DIRECTION ( 'NONE',  ( 0.000000000000000000, -0.2697967711570115057, -0.9629172873478029082 ) ) ;
#3053 = DIRECTION ( 'NONE',  ( -6.123233995736816572E-17, -1.060575238724904203E-16, -1.000000000000000000 ) ) ;
#3054 = CARTESIAN_POINT ( 'NONE',  ( -16.62983158603122646, -6.888301780572501976, -19.69301249981969448 ) ) ;
#3055 = CARTESIAN_POINT ( 'NONE',  ( -9.015947181032835626E-10, -7.500000000000007994, -19.28004999981968481 ) ) ;
#3056 = DIRECTION ( 'NONE',  ( 0.000000000000000000, 0.000000000000000000, 1.000000000000000000 ) ) ;
#3057 = CARTESIAN_POINT ( 'NONE',  ( 13.67243654778934925, 5.663308646854335215, 9.533145581519077538 ) ) ;
#3058 = EDGE_CURVE ( 'NONE', #9385, #10906, #5062, .T. ) ;
#3059 = CARTESIAN_POINT ( 'NONE',  ( 19.99999999999999645, 10.74906464462217848, -71.19310085447956737 ) ) ;
#3060 = VERTEX_POINT ( 'NONE', #19683 ) ;
#3061 = CARTESIAN_POINT ( 'NONE',  ( 19.99999999999999645, -27.62776854598897813, 58.65812137498992485 ) ) ;
#3062 = CARTESIAN_POINT ( 'NONE',  ( 15.25966317163202746, 10.19618095047498407, -15.27504374981969093 ) ) ;
#3063 = DIRECTION ( 'NONE',  ( -1.000000000000000000, 0.000000000000000000, 0.000000000000000000 ) ) ;
#3064 = VERTEX_POINT ( 'NONE', #11842 ) ;
#3065 = DIRECTION ( 'NONE',  ( 0.000000000000000000, 0.000000000000000000, 1.000000000000000000 ) ) ;
#3066 = ORIENTED_EDGE ( 'NONE', *, *, #15195, .F. ) ;
#3067 = DIRECTION ( 'NONE',  ( 0.000000000000000000, 0.3984010898462361228, 0.9172113015054552676 ) ) ;
#3068 = CARTESIAN_POINT ( 'NONE',  ( 0.000000000000000000, 0.000000000000000000, 46.00000000000000711 ) ) ;
#3069 = AXIS2_PLACEMENT_3D ( 'NONE', #13931, #14247, #17221 ) ;
#3070 = EDGE_LOOP ( 'NONE', ( #10488, #17439, #828, #19141 ) ) ;
#3071 = ORIENTED_EDGE ( 'NONE', *, *, #9944, .F. ) ;
#3072 = CARTESIAN_POINT ( 'NONE',  ( 50.00000000000000000, -164.9999999999999716, 90.00000000000001421 ) ) ;
#3073 = VECTOR ( 'NONE', #3820, 1000.000000000000000 ) ;
#3074 = AXIS2_PLACEMENT_3D ( 'NONE', #466, #9793, #4921 ) ;
#3075 = SURFACE_STYLE_USAGE ( .BOTH. , #9333 ) ;
#3076 = DIRECTION ( 'NONE',  ( 0.000000000000000000, 0.000000000000000000, 1.000000000000000000 ) ) ;
#3077 = CARTESIAN_POINT ( 'NONE',  ( 0.2500000000000002220, 0.000000000000000000, 0.000000000000000000 ) ) ;
#3078 = CARTESIAN_POINT ( 'NONE',  ( 11.17563879758428769, 2.222972768810838939, -12.07692149935257397 ) ) ;
#3079 = CARTESIAN_POINT ( 'NONE',  ( 2.222972771497739419, 11.17563879704981922, 16.73317149971319751 ) ) ;
#3080 = EDGE_CURVE ( 'NONE', #297, #7334, #620, .T. ) ;
#3081 = DIRECTION ( 'NONE',  ( 0.000000000000000000, 0.5195839500354287877, 0.8544194045464914566 ) ) ;
#3082 = DIRECTION ( 'NONE',  ( -0.000000000000000000, -0.000000000000000000, -1.000000000000000000 ) ) ;
#3083 = FACE_OUTER_BOUND ( 'NONE', #3496, .T. ) ;
#3084 = ORIENTED_EDGE ( 'NONE', *, *, #2866, .F. ) ;
#3085 = CARTESIAN_POINT ( 'NONE',  ( 0.000000000000000000, 0.000000000000000000, 81.99999999999998579 ) ) ;
#3086 = EDGE_LOOP ( 'NONE', ( #914, #19433, #10017, #15743 ) ) ;
#3087 = CARTESIAN_POINT ( 'NONE',  ( -3.580422614997675002, -17.99999999956958163, -13.64526874981969229 ) ) ;
#3088 = DIRECTION ( 'NONE',  ( -0.000000000000000000, 0.000000000000000000, 1.000000000000000000 ) ) ;
#3089 = AXIS2_PLACEMENT_3D ( 'NONE', #8275, #3498, #16138 ) ;
#3090 = ADVANCED_FACE ( 'NONE', ( #14830 ), #11947, .T. ) ;
#3091 = ORIENTED_EDGE ( 'NONE', *, *, #5199, .T. ) ;
#3092 = EDGE_CURVE ( 'NONE', #10942, #8932, #4499, .T. ) ;
#3093 = DIRECTION ( 'NONE',  ( 0.000000000000000000, 0.000000000000000000, -1.000000000000000000 ) ) ;
#3094 = EDGE_LOOP ( 'NONE', ( #5989, #19536 ) ) ;
#3095 = CARTESIAN_POINT ( 'NONE',  ( 1.491842754445842578, -7.500000000179340987, -6.989481249819691655 ) ) ;
#3096 = CARTESIAN_POINT ( 'NONE',  ( 10.00000000000000178, -164.9999999999999716, 66.80000000000001137 ) ) ;
#3097 = DIRECTION ( 'NONE',  ( 1.000000000000000000, 1.836909530733573776E-16, 0.000000000000000000 ) ) ;
#3098 = AXIS2_PLACEMENT_3D ( 'NONE', #10998, #10583, #12494 ) ;
#3099 = ORIENTED_EDGE ( 'NONE', *, *, #16627, .T. ) ;
#3100 = CYLINDRICAL_SURFACE ( 'NONE', #5265, 10.00000000000000178 ) ;
#3101 = DIRECTION ( 'NONE',  ( -0.5000000000000037748, -0.8660254037844364872, 0.000000000000000000 ) ) ;
#3102 = FACE_OUTER_BOUND ( 'NONE', #11979, .T. ) ;
#3103 = DIRECTION ( 'NONE',  ( 1.000000000000000000, -0.000000000000000000, -0.000000000000000000 ) ) ;
#3104 = VECTOR ( 'NONE', #12705, 1000.000000000000000 ) ;
#3105 = ORIENTED_EDGE ( 'NONE', *, *, #15117, .T. ) ;
#3106 = CARTESIAN_POINT ( 'NONE',  ( 0.000000000000000000, -1.178949249685214307, 2.042000000000001592 ) ) ;
#3107 = VERTEX_POINT ( 'NONE', #18107 ) ;
#3108 = CIRCLE ( 'NONE', #20696, 10.85999999999999410 ) ;
#3109 = DIRECTION ( 'NONE',  ( -0.000000000000000000, -1.000000000000000000, -0.000000000000000000 ) ) ;
#3110 = DIRECTION ( 'NONE',  ( 1.000000000000000000, -0.000000000000000000, -0.000000000000000000 ) ) ;
#3111 = EDGE_LOOP ( 'NONE', ( #1091, #16142, #17240, #7839, #9407 ) ) ;
#3112 = LINE ( 'NONE', #7996, #16631 ) ;
#3113 = CARTESIAN_POINT ( 'NONE',  ( 0.000000000000000000, -27.80658314415180499, -66.41380830714152239 ) ) ;
#3114 = CARTESIAN_POINT ( 'NONE',  ( 0.000000000000000000, 0.000000000000000000, 68.00000000000000000 ) ) ;
#3115 = AXIS2_PLACEMENT_3D ( 'NONE', #15849, #1343, #14261 ) ;
#3116 = VERTEX_POINT ( 'NONE', #11745 ) ;
#3117 = EDGE_CURVE ( 'NONE', #19897, #1468, #423, .T. ) ;
#3118 = CIRCLE ( 'NONE', #8854, 72.00000000007199219 ) ;
#3119 = CARTESIAN_POINT ( 'NONE',  ( 3.600000000000066702, 10.82531754730546147, 46.00000000000000711 ) ) ;
#3120 = ORIENTED_EDGE ( 'NONE', *, *, #19475, .T. ) ;
#3121 = CARTESIAN_POINT ( 'NONE',  ( 6.249999999999902300, -10.82531754730554496, 166.0000000000000000 ) ) ;
#3122 = EDGE_CURVE ( 'NONE', #10495, #16164, #19056, .T. ) ;
#3123 = ORIENTED_EDGE ( 'NONE', *, *, #11908, .T. ) ;
#3124 = EDGE_CURVE ( 'NONE', #6246, #13015, #13974, .T. ) ;
#3125 = CARTESIAN_POINT ( 'NONE',  ( 50.00000000000000000, 31.35083268962919689, -84.99999999999998579 ) ) ;
#3126 = DIRECTION ( 'NONE',  ( -0.000000000000000000, -0.000000000000000000, 1.000000000000000000 ) ) ;
#3127 = CARTESIAN_POINT ( 'NONE',  ( -14.79893867793684059, -2.943691925285399691, -17.54173933115846040 ) ) ;
#3128 = AXIS2_PLACEMENT_3D ( 'NONE', #12388, #13980, #4222 ) ;
#3130 = VERTEX_POINT ( 'NONE', #11526 ) ;
#3129 = CIRCLE ( 'NONE', #5830, 2.099999999999997868 ) ;
#3131 = DIRECTION ( 'NONE',  ( 0.000000000000000000, 0.9790840876823234673, -0.2034560130526308908 ) ) ;
#3132 = DIRECTION ( 'NONE',  ( 0.000000000000000000, 0.5000000000000009992, 0.8660254037844380415 ) ) ;
#3133 = AXIS2_PLACEMENT_3D ( 'NONE', #20209, #6016, #5686 ) ;
#3134 = ORIENTED_EDGE ( 'NONE', *, *, #13123, .T. ) ;
#3135 = CARTESIAN_POINT ( 'NONE',  ( -0.7462824556787200914, -21.49896008043337403, 76.04131803729603689 ) ) ;
#3136 = EDGE_CURVE ( 'NONE', #200, #2521, #7064, .T. ) ;
#3137 = FACE_OUTER_BOUND ( 'NONE', #19583, .T. ) ;
#3138 = DIRECTION ( 'NONE',  ( 1.000000000000000000, 0.000000000000000000, 0.000000000000000000 ) ) ;
#3139 = DIRECTION ( 'NONE',  ( -1.000000000000000000, -0.000000000000000000, -0.000000000000000000 ) ) ;
#3140 = EDGE_CURVE ( 'NONE', #3060, #16924, #6188, .T. ) ;
#3141 = ORIENTED_EDGE ( 'NONE', *, *, #15957, .F. ) ;
#3142 = EDGE_CURVE ( 'NONE', #20917, #2697, #13449, .T. ) ;
#3143 = DIRECTION ( 'NONE',  ( -1.000000000000000000, 0.000000000000000000, 0.000000000000000000 ) ) ;
#3144 = CARTESIAN_POINT ( 'NONE',  ( 8.899999999999902656, -10.82531754730554496, 43.00000000000000000 ) ) ;
#3145 = ORIENTED_EDGE ( 'NONE', *, *, #13625, .F. ) ;
#3146 = CIRCLE ( 'NONE', #17357, 72.00000000007199219 ) ;
#3147 = CARTESIAN_POINT ( 'NONE',  ( 0.000000000000000000, 0.000000000000000000, 81.99999999999998579 ) ) ;
#3148 = VECTOR ( 'NONE', #8243, 1000.000000000000000 ) ;
#3149 = CARTESIAN_POINT ( 'NONE',  ( 1.318516776095788545, 3.857556137907071747, -5.600000000000003197 ) ) ;
#3150 = ADVANCED_FACE ( 'NONE', ( #302 ), #18367, .F. ) ;
#3151 = CYLINDRICAL_SURFACE ( 'NONE', #1811, 17.50000000000000355 ) ;
#3152 = EDGE_LOOP ( 'NONE', ( #2943, #6034, #6957, #14481 ) ) ;
#3153 = PLANE ( 'NONE',  #18184 ) ;
#3154 = CARTESIAN_POINT ( 'NONE',  ( 43.62500077266425791, -125.0000000000000000, 90.00000000000002842 ) ) ;
#3155 = CARTESIAN_POINT ( 'NONE',  ( 30.00000000000000000, 0.000000000000000000, 0.000000000000000000 ) ) ;
#3156 = AXIS2_PLACEMENT_3D ( 'NONE', #18774, #7630, #1071 ) ;
#3157 = CARTESIAN_POINT ( 'NONE',  ( 15.25966317163203101, 10.19618095047498585, -15.27504374981969448 ) ) ;
#3158 = AXIS2_PLACEMENT_3D ( 'NONE', #862, #3709, #18455 ) ;
#3159 = DIRECTION ( 'NONE',  ( 1.000000000000000000, -0.000000000000000000, -0.000000000000000000 ) ) ;
#3160 = TOROIDAL_SURFACE ( 'NONE', #11960, 2.700000000000000622, 0.2000000000000000111 ) ;
#3161 = CARTESIAN_POINT ( 'NONE',  ( 9.999999999999998224, -27.80658314415272159, 66.41380830714115291 ) ) ;
#3162 = AXIS2_PLACEMENT_3D ( 'NONE', #6497, #13703, #6914 ) ;
#3163 = ADVANCED_FACE ( 'NONE', ( #6753 ), #6961, .T. ) ;
#3164 = CARTESIAN_POINT ( 'NONE',  ( -1.779019326032424095E-09, -14.79893867758296544, -6.371541918480928324 ) ) ;
#3165 = EDGE_CURVE ( 'NONE', #9669, #6207, #1799, .T. ) ;
#3166 = DIRECTION ( 'NONE',  ( 0.000000000000000000, 1.000000000000000000, -3.469446951953615175E-16 ) ) ;
#3167 = APPLICATION_CONTEXT ( 'automotive_design' ) ;
#3168 = ORIENTED_EDGE ( 'NONE', *, *, #1952, .T. ) ;
#3169 = DIRECTION ( 'NONE',  ( 0.000000000000000000, 0.000000000000000000, 1.000000000000000000 ) ) ;
#3170 = EDGE_CURVE ( 'NONE', #19379, #11771, #20719, .T. ) ;
#3171 = LINE ( 'NONE', #3572, #6644 ) ;
#3172 = FACE_OUTER_BOUND ( 'NONE', #9902, .T. ) ;
#3173 = VECTOR ( 'NONE', #11996, 1000.000000000000000 ) ;
#3174 = ORIENTED_EDGE ( 'NONE', *, *, #19914, .F. ) ;
#3175 = AXIS2_PLACEMENT_3D ( 'NONE', #14733, #6454, #207 ) ;
#3176 = DIRECTION ( 'NONE',  ( 1.000000000000000000, -0.000000000000000000, -0.000000000000000000 ) ) ;
#3177 = ORIENTED_EDGE ( 'NONE', *, *, #19190, .T. ) ;
#3178 = CARTESIAN_POINT ( 'NONE',  ( 43.01509889268501752, -11.40594424968584519, -82.27917910797492596 ) ) ;
#3179 = CARTESIAN_POINT ( 'NONE',  ( 5.000000000000002665, 0.000000000000000000, -2.700000000000000622 ) ) ;
#3180 = VERTEX_POINT ( 'NONE', #5789 ) ;
#3181 = ORIENTED_EDGE ( 'NONE', *, *, #15051, .T. ) ;
#3182 = DIRECTION ( 'NONE',  ( 1.000000000000000000, 1.836909530733573776E-16, 0.000000000000000000 ) ) ;
#3183 = CIRCLE ( 'NONE', #2845, 0.2500000000000002220 ) ;
#3184 = EDGE_CURVE ( 'NONE', #4504, #19648, #4420, .T. ) ;
#3185 = PRESENTATION_STYLE_ASSIGNMENT (( #19093 ) ) ;
#3186 = CARTESIAN_POINT ( 'NONE',  ( 30.00000000000000000, -85.00000000000000000, -1.040949779275250179E-14 ) ) ;
#3187 = SURFACE_SIDE_STYLE ('',( #11454 ) ) ;
#3188 = CARTESIAN_POINT ( 'NONE',  ( 6.358192987158595599, -4.248408730893249441, 16.94729375018031803 ) ) ;
#3189 = AXIS2_PLACEMENT_3D ( 'NONE', #11060, #4380, #6174 ) ;
#3190 = CARTESIAN_POINT ( 'NONE',  ( 7.902369976724389566, -7.902369978624323110, 1.123015249713196217 ) ) ;
#3191 = CARTESIAN_POINT ( 'NONE',  ( -32.96694501150314949, -24.74873734152930993, -120.0000000000000142 ) ) ;
#3192 = CARTESIAN_POINT ( 'NONE',  ( 30.00000000000000000, -159.9999999999999716, 53.99496054166689873 ) ) ;
#3193 = CARTESIAN_POINT ( 'NONE',  ( 0.000000000000000000, 0.000000000000000000, 40.00000000000000000 ) ) ;
#3194 = AXIS2_PLACEMENT_3D ( 'NONE', #3627, #6800, #6493 ) ;
#3195 = ORIENTED_EDGE ( 'NONE', *, *, #11286, .F. ) ;
#3196 = FACE_OUTER_BOUND ( 'NONE', #3994, .T. ) ;
#3197 = EDGE_LOOP ( 'NONE', ( #10519, #16434, #13543, #5712, #6919 ) ) ;
#3198 = CARTESIAN_POINT ( 'NONE',  ( 6.888301784570728614, 16.62983158437510056, 21.54136250018031618 ) ) ;
#3199 = CARTESIAN_POINT ( 'NONE',  ( 19.99999999999999645, -70.68211945903178162, -13.71269443944282074 ) ) ;
#3200 = ORIENTED_EDGE ( 'NONE', *, *, #17105, .F. ) ;
#3201 = DIRECTION ( 'NONE',  ( 0.000000000000000000, 0.000000000000000000, 1.000000000000000000 ) ) ;
#3202 = EDGE_LOOP ( 'NONE', ( #18416, #16778, #6482, #10806 ) ) ;
#3203 = CARTESIAN_POINT ( 'NONE',  ( 0.000000000000000000, 0.000000000000000000, 0.000000000000000000 ) ) ;
#3204 = CARTESIAN_POINT ( 'NONE',  ( 0.000000000000000000, 15.58726123847937828, -62.93731870009387563 ) ) ;
#3205 = ORIENTED_EDGE ( 'NONE', *, *, #18428, .F. ) ;
#3206 = VERTEX_POINT ( 'NONE', #17254 ) ;
#3207 = CARTESIAN_POINT ( 'NONE',  ( 10.00000000000000178, -160.0000000000000000, 73.20000000000000284 ) ) ;
#3208 = EDGE_CURVE ( 'NONE', #15761, #6177, #15544, .T. ) ;
#3209 = ADVANCED_FACE ( 'NONE', ( #13757 ), #16925, .T. ) ;
#3210 = CARTESIAN_POINT ( 'NONE',  ( -12.50000000000000533, 0.000000000000000000, 43.00000000000000000 ) ) ;
#3211 = CARTESIAN_POINT ( 'NONE',  ( 4.000000000000003553, 2.309401076758524685, -0.3572655899081733644 ) ) ;
#3212 = VECTOR ( 'NONE', #14447, 1000.000000000000000 ) ;
#3213 = PLANE ( 'NONE',  #9610 ) ;
#3214 = ORIENTED_EDGE ( 'NONE', *, *, #5337, .T. ) ;
#3215 = DIRECTION ( 'NONE',  ( 0.000000000000000000, 0.000000000000000000, 1.000000000000000000 ) ) ;
#3216 = DIRECTION ( 'NONE',  ( -1.000000000000000000, 0.000000000000000000, 0.000000000000000000 ) ) ;
#3217 = CARTESIAN_POINT ( 'NONE',  ( -7.500000000000009770, 9.706494107251932559E-15, 1.926200000002316060 ) ) ;
#3218 = PLANE ( 'NONE',  #15694 ) ;
#3219 = AXIS2_PLACEMENT_3D ( 'NONE', #1515, #16322, #13250 ) ;
#3220 = VERTEX_POINT ( 'NONE', #1040 ) ;
#3221 = DIRECTION ( 'NONE',  ( -1.000000000000000000, -0.000000000000000000, -0.000000000000000000 ) ) ;
#3222 = CARTESIAN_POINT ( 'NONE',  ( 19.99999999999999645, 5.762283366692075859, -64.99406197038663890 ) ) ;
#3223 = DIRECTION ( 'NONE',  ( -1.000000000000000000, 0.000000000000000000, 0.000000000000000000 ) ) ;
#3224 = ORIENTED_EDGE ( 'NONE', *, *, #19175, .F. ) ;
#3225 = FACE_BOUND ( 'NONE', #10330, .T. ) ;
#3226 = ORIENTED_EDGE ( 'NONE', *, *, #19984, .T. ) ;
#3227 = AXIS2_PLACEMENT_3D ( 'NONE', #726, #3589, #527 ) ;
#3228 = DIRECTION ( 'NONE',  ( -1.000000000000000000, 0.000000000000000000, 0.000000000000000000 ) ) ;
#3229 = ORIENTED_EDGE ( 'NONE', *, *, #5893, .F. ) ;
#3230 = CARTESIAN_POINT ( 'NONE',  ( -10.00000000000000000, 0.000000000000000000, 0.000000000000000000 ) ) ;
#3231 = DIRECTION ( 'NONE',  ( 1.000000000000000000, 0.000000000000000000, 0.000000000000000000 ) ) ;
#3232 = CARTESIAN_POINT ( 'NONE',  ( -7.902369976724401113, 7.902369978624329327, 22.38323475064743562 ) ) ;
#3233 = ADVANCED_FACE ( 'NONE', ( #20533 ), #17359, .T. ) ;
#3234 = EDGE_LOOP ( 'NONE', ( #14699, #18134, #8606, #15597 ) ) ;
#3235 = AXIS2_PLACEMENT_3D ( 'NONE', #8186, #19832, #14759 ) ;
#3236 = DIRECTION ( 'NONE',  ( -1.000000000000000000, 0.000000000000000000, -0.000000000000000000 ) ) ;
#3237 = PLANE ( 'NONE',  #779 ) ;
#3238 = ORIENTED_EDGE ( 'NONE', *, *, #11240, .F. ) ;
#3239 = DIRECTION ( 'NONE',  ( -1.000000000000000000, 0.000000000000000000, 0.000000000000000000 ) ) ;
#3240 = CARTESIAN_POINT ( 'NONE',  ( -12.72792205982779912, 12.72792206288790950, 19.77417500018031404 ) ) ;
#3241 = CYLINDRICAL_SURFACE ( 'NONE', #10061, 35.00000000000000000 ) ;
#3242 = CARTESIAN_POINT ( 'NONE',  ( 5.200000000000002842, 0.000000000000000000, 0.000000000000000000 ) ) ;
#3243 = EDGE_CURVE ( 'NONE', #5413, #2556, #9980, .T. ) ;
#3244 = EDGE_LOOP ( 'NONE', ( #2384, #19639, #15365, #13230 ) ) ;
#3245 = AXIS2_PLACEMENT_3D ( 'NONE', #17678, #16085, #8029 ) ;
#3246 = CARTESIAN_POINT ( 'NONE',  ( -17.50000000000000355, 2.143131898507868643E-15, 126.0000000000000000 ) ) ;
#3247 = VERTEX_POINT ( 'NONE', #16084 ) ;
#3248 = CARTESIAN_POINT ( 'NONE',  ( -10.00000000000000000, 0.000000000000000000, 0.000000000000000000 ) ) ;
#3249 = AXIS2_PLACEMENT_3D ( 'NONE', #15106, #1865, #5247 ) ;
#3250 = CIRCLE ( 'NONE', #18829, 2.041999999999999815 ) ;
#3251 = DIRECTION ( 'NONE',  ( -1.000000000000000000, 0.000000000000000000, -0.000000000000000000 ) ) ;
#3252 = CARTESIAN_POINT ( 'NONE',  ( 5.303300859536635770, 5.303300858261589923, -3.964424999819686324 ) ) ;
#3253 = ORIENTED_EDGE ( 'NONE', *, *, #4985, .F. ) ;
#3254 = CARTESIAN_POINT ( 'NONE',  ( 2.500000000000000000, -2.357898499370432166, 3.035766082959412415E-15 ) ) ;
#3255 = CIRCLE ( 'NONE', #17825, 17.50000000000000355 ) ;
#3256 = FACE_OUTER_BOUND ( 'NONE', #2487, .T. ) ;
#3257 = DIRECTION ( 'NONE',  ( 1.760777620558074541E-30, -1.056873212472353686E-31, 1.000000000000000000 ) ) ;
#3258 = CARTESIAN_POINT ( 'NONE',  ( -12.72792206288791483, -12.72792205982780089, -10.85707499981969448 ) ) ;
#3259 = EDGE_CURVE ( 'NONE', #8741, #1553, #17004, .T. ) ;
#3260 = ORIENTED_EDGE ( 'NONE', *, *, #18428, .T. ) ;
#3261 = CIRCLE ( 'NONE', #13748, 17.50000000000000355 ) ;
#3262 = ADVANCED_FACE ( 'NONE', ( #1572 ), #14287, .T. ) ;
#3263 = DIRECTION ( 'NONE',  ( 1.000000000000000000, 0.000000000000000000, 0.000000000000000000 ) ) ;
#3264 = DIRECTION ( 'NONE',  ( 0.000000000000000000, 0.000000000000000000, -1.000000000000000000 ) ) ;
#3265 = AXIS2_PLACEMENT_3D ( 'NONE', #7683, #15622, #9583 ) ;
#3266 = AXIS2_PLACEMENT_3D ( 'NONE', #19153, #12479, #4834 ) ;
#3267 = CARTESIAN_POINT ( 'NONE',  ( -12.54593441764187034, -8.382925368423267187, -4.898885668480925659 ) ) ;
#3268 =( GEOMETRIC_REPRESENTATION_CONTEXT ( 3 ) GLOBAL_UNCERTAINTY_ASSIGNED_CONTEXT ( ( #3689 ) ) GLOBAL_UNIT_ASSIGNED_CONTEXT ( ( #10185, #9871, #10087 ) ) REPRESENTATION_CONTEXT ( 'NONE', 'WORKASPACE' ) );
#3269 = CARTESIAN_POINT ( 'NONE',  ( 19.99999999999999645, -60.35829202194891252, 24.78524934717529504 ) ) ;
#3270 = ADVANCED_FACE ( 'NONE', ( #11413 ), #14595, .F. ) ;
#3271 = VERTEX_POINT ( 'NONE', #13011 ) ;
#3272 = DIRECTION ( 'NONE',  ( 0.000000000000000000, -0.9976687691905398170, 0.06824241336466072005 ) ) ;
#3273 = CIRCLE ( 'NONE', #10034, 27.60000000002759535 ) ;
#3274 = CARTESIAN_POINT ( 'NONE',  ( -31.75000000000000000, 0.000000000000000000, 0.000000000000000000 ) ) ;
#3275 = LINE ( 'NONE', #3466, #18526 ) ;
#3276 = ORIENTED_EDGE ( 'NONE', *, *, #7027, .F. ) ;
#3277 = CARTESIAN_POINT ( 'NONE',  ( 19.99999999999999645, -56.42118728228132341, -32.77318456705499017 ) ) ;
#3278 = CIRCLE ( 'NONE', #19524, 65.24900000006525147 ) ;
#3279 = ORIENTED_EDGE ( 'NONE', *, *, #4958, .T. ) ;
#3280 = CARTESIAN_POINT ( 'NONE',  ( 0.000000000000000000, -60.35829202194857857, -24.78524934717611572 ) ) ;
#3281 = CARTESIAN_POINT ( 'NONE',  ( -16.62983158603121936, -6.888301780572499311, 16.10238750018030984 ) ) ;
#3282 = CIRCLE ( 'NONE', #11403, 27.60000000002760601 ) ;
#3283 = ORIENTED_EDGE ( 'NONE', *, *, #19521, .T. ) ;
#3284 = EDGE_CURVE ( 'NONE', #2910, #19113, #11927, .T. ) ;
#3285 = ORIENTED_EDGE ( 'NONE', *, *, #16985, .T. ) ;
#3286 = DIRECTION ( 'NONE',  ( -1.000000000000000000, -0.000000000000000000, -0.000000000000000000 ) ) ;
#3287 = ADVANCED_FACE ( 'NONE', ( #8028 ), #20942, .T. ) ;
#3288 = AXIS2_PLACEMENT_3D ( 'NONE', #4941, #6418, #14592 ) ;
#3289 =( GEOMETRIC_REPRESENTATION_CONTEXT ( 3 ) GLOBAL_UNCERTAINTY_ASSIGNED_CONTEXT ( ( #3895 ) ) GLOBAL_UNIT_ASSIGNED_CONTEXT ( ( #15899, #14325, #11028 ) ) REPRESENTATION_CONTEXT ( 'NONE', 'WORKASPACE' ) );
#3290 = DIRECTION ( 'NONE',  ( -1.000000000000000000, 0.000000000000000000, 0.000000000000000000 ) ) ;
#3291 = DIRECTION ( 'NONE',  ( -0.000000000000000000, -0.000000000000000000, 1.000000000000000000 ) ) ;
#3292 = ADVANCED_FACE ( 'NONE', ( #15969 ), #14190, .F. ) ;
#3293 = DIRECTION ( 'NONE',  ( -0.000000000000000000, -0.000000000000000000, 1.000000000000000000 ) ) ;
#3294 = CARTESIAN_POINT ( 'NONE',  ( -2.870125741905213079, 6.929096494179683319, 22.54338750018031590 ) ) ;
#3295 = VECTOR ( 'NONE', #14523, 1000.000000000000000 ) ;
#3296 = CARTESIAN_POINT ( 'NONE',  ( 6.330490858644138186, 9.474249097082495297, -1.527766000286801873 ) ) ;
#3297 = CIRCLE ( 'NONE', #13102, 17.50000000000000355 ) ;
#3298 = DIRECTION ( 'NONE',  ( -1.000000000000000000, -0.000000000000000000, -0.000000000000000000 ) ) ;
#3299 = CARTESIAN_POINT ( 'NONE',  ( 50.00100000000000477, -85.00000000000000000, 8.999999999999984013 ) ) ;
#3300 = DIRECTION ( 'NONE',  ( 0.000000000000000000, 0.000000000000000000, -1.000000000000000000 ) ) ;
#3301 = AXIS2_PLACEMENT_3D ( 'NONE', #20681, #14136, #4475 ) ;
#3302 = VERTEX_POINT ( 'NONE', #11312 ) ;
#3303 = AXIS2_PLACEMENT_3D ( 'NONE', #424, #20120, #11970 ) ;
#3304 = CARTESIAN_POINT ( 'NONE',  ( 0.000000000000000000, 0.000000000000000000, 40.00000000000000000 ) ) ;
#3305 = CARTESIAN_POINT ( 'NONE',  ( -17.99999999956958519, 3.580422614997674113, 18.89058125018031120 ) ) ;
#3306 = DIRECTION ( 'NONE',  ( -1.000000000000000000, 0.000000000000000000, 0.000000000000000000 ) ) ;
#3307 = VERTEX_POINT ( 'NONE', #6110 ) ;
#3308 = PLANE ( 'NONE',  #5517 ) ;
#3309 = VERTEX_POINT ( 'NONE', #70 ) ;
#3310 = CYLINDRICAL_SURFACE ( 'NONE', #14265, 2.500000000000000444 ) ;
#3311 = DIRECTION ( 'NONE',  ( 1.000000000000000000, 1.836909530733573776E-16, 0.000000000000000000 ) ) ;
#3312 = ORIENTED_EDGE ( 'NONE', *, *, #17259, .F. ) ;
#3313 = AXIS2_PLACEMENT_3D ( 'NONE', #1035, #7484, #9299 ) ;
#3314 = ORIENTED_EDGE ( 'NONE', *, *, #10940, .T. ) ;
#3315 = CARTESIAN_POINT ( 'NONE',  ( 0.000000000000000000, -0.9548212943360432359, -71.99366858485717557 ) ) ;
#3316 = VECTOR ( 'NONE', #4614, 1000.000000000000000 ) ;
#3317 = CARTESIAN_POINT ( 'NONE',  ( 2.681483223904246760, -3.070647092368467668, -2.072929885643508434E-14 ) ) ;
#3318 = COLOUR_RGB ( '', 0.31764706, 0.68627451, 0.89019608) ;
#3319 = DIRECTION ( 'NONE',  ( -1.000000000000000000, -0.000000000000000000, 0.000000000000000000 ) ) ;
#3320 = ORIENTED_EDGE ( 'NONE', *, *, #16116, .F. ) ;
#3321 = CARTESIAN_POINT ( 'NONE',  ( -2.870125743571140919, -6.929096493489624642, 12.74411250018031261 ) ) ;
#3322 = CARTESIAN_POINT ( 'NONE',  ( -4.248408730893249441, -6.358192987158596488, 0.4535437501803143978 ) ) ;
#3323 = DIRECTION ( 'NONE',  ( 0.000000000000000000, 0.9976687691905390398, 0.06824241336467466723 ) ) ;
#3324 = DIRECTION ( 'NONE',  ( 1.000000000000000000, 0.000000000000000000, -0.000000000000000000 ) ) ;
#3325 = EDGE_LOOP ( 'NONE', ( #16902, #6501, #18915, #14151, #7043 ) ) ;
#3326 = ADVANCED_FACE ( 'NONE', ( #17784 ), #15869, .T. ) ;
#3327 = CARTESIAN_POINT ( 'NONE',  ( -7.500000000000000000, 0.000000000000000000, 40.00000000000000000 ) ) ;
#3328 = DIRECTION ( 'NONE',  ( 1.000000000000000000, 1.836909530733573776E-16, 0.000000000000000000 ) ) ;
#3329 = DIRECTION ( 'NONE',  ( 0.000000000000000000, 0.000000000000000000, 1.000000000000000000 ) ) ;
#3330 = ORIENTED_EDGE ( 'NONE', *, *, #6200, .F. ) ;
#3331 = DIRECTION ( 'NONE',  ( -1.000000000000000000, 0.000000000000000000, 0.000000000000000000 ) ) ;
#3332 = ORIENTED_EDGE ( 'NONE', *, *, #14716, .T. ) ;
#3333 = CYLINDRICAL_SURFACE ( 'NONE', #3074, 2.649999999999993694 ) ;
#3334 = VERTEX_POINT ( 'NONE', #2944 ) ;
#3335 = DIRECTION ( 'NONE',  ( -1.000000000000000000, 0.000000000000000000, 0.000000000000000000 ) ) ;
#3336 = CARTESIAN_POINT ( 'NONE',  ( 10.00000000000000178, -164.9999999999999716, -66.80000000000001137 ) ) ;
#3337 = CARTESIAN_POINT ( 'NONE',  ( 13.67243654642775574, -5.663308650141541278, -11.94564558115845898 ) ) ;
#3338 = VERTEX_POINT ( 'NONE', #1365 ) ;
#3339 = FACE_OUTER_BOUND ( 'NONE', #16825, .T. ) ;
#3340 = DIRECTION ( 'NONE',  ( -1.000000000000000000, 0.000000000000000000, 0.000000000000000000 ) ) ;
#3341 = ORIENTED_EDGE ( 'NONE', *, *, #10133, .F. ) ;
#3342 = CARTESIAN_POINT ( 'NONE',  ( -19.93133741578929730, -8.067442883292189393, -78.55234307929258364 ) ) ;
#3343 = EDGE_CURVE ( 'NONE', #10522, #405, #3046, .T. ) ;
#3344 = CARTESIAN_POINT ( 'NONE',  ( -31.74999999999995737, 0.000000000000000000, 0.000000000000000000 ) ) ;
#3345 = CARTESIAN_POINT ( 'NONE',  ( 19.99999999999999645, 48.70996102988680576, 42.79495875147792106 ) ) ;
#3346 = FACE_OUTER_BOUND ( 'NONE', #4811, .T. ) ;
#3347 = ORIENTED_EDGE ( 'NONE', *, *, #5149, .T. ) ;
#3348 = DIRECTION ( 'NONE',  ( -1.000000000000000000, -0.000000000000000000, 0.000000000000000000 ) ) ;
#3349 = ORIENTED_EDGE ( 'NONE', *, *, #14687, .T. ) ;
#3350 = EDGE_CURVE ( 'NONE', #10983, #18697, #19703, .T. ) ;
#3351 = DIRECTION ( 'NONE',  ( 0.000000000000000000, 0.000000000000000000, 1.000000000000000000 ) ) ;
#3352 = CARTESIAN_POINT ( 'NONE',  ( 19.99999999999999645, -43.56693332842751687, -48.57318520917550586 ) ) ;
#3353 = CARTESIAN_POINT ( 'NONE',  ( 6.999999999999999112, 7.118024431592597790E-15, 0.000000000000000000 ) ) ;
#3354 = ORIENTED_EDGE ( 'NONE', *, *, #18282, .F. ) ;
#3355 = CYLINDRICAL_SURFACE ( 'NONE', #2952, 27.60000000002760245 ) ;
#3356 = CARTESIAN_POINT ( 'NONE',  ( -30.00000000000000000, -85.00000000000000000, 11.49999999999998579 ) ) ;
#3357 = CARTESIAN_POINT ( 'NONE',  ( 6.250000000000201617, 10.82531754730537799, -39.99999999999999289 ) ) ;
#3358 = CARTESIAN_POINT ( 'NONE',  ( -6.888301780572502864, 16.62983158603122646, -7.911762499819691818 ) ) ;
#3359 = ORIENTED_EDGE ( 'NONE', *, *, #9567, .T. ) ;
#3360 = CARTESIAN_POINT ( 'NONE',  ( 6.929096494179677990, 2.870125741905210859, 9.209737500180310121 ) ) ;
#3361 = DIRECTION ( 'NONE',  ( 0.000000000000000000, 0.000000000000000000, 1.000000000000000000 ) ) ;
#3362 = CARTESIAN_POINT ( 'NONE',  ( -8.382925371439625906, -12.54593441562639988, 3.937051831519074341 ) ) ;
#3363 = DIRECTION ( 'NONE',  ( 0.000000000000000000, 1.000000000000000000, 0.000000000000000000 ) ) ;
#3364 = ORIENTED_EDGE ( 'NONE', *, *, #17671, .F. ) ;
#3365 = DIRECTION ( 'NONE',  ( -1.000000000000000000, 0.000000000000000000, 0.000000000000000000 ) ) ;
#3366 = CARTESIAN_POINT ( 'NONE',  ( 24.99999999999999289, -110.0000000000000142, 44.99999999999999289 ) ) ;
#3367 = CARTESIAN_POINT ( 'NONE',  ( 43.03985923310276007, -11.23385978448955136, 76.06858800491698958 ) ) ;
#3368 = EDGE_LOOP ( 'NONE', ( #1791, #9990, #13865, #20173, #2812, #9966 ) ) ;
#3369 = EDGE_CURVE ( 'NONE', #13140, #11331, #10580, .T. ) ;
#3370 = CARTESIAN_POINT ( 'NONE',  ( 19.99999999999999645, -64.80702306891090814, -7.581672767547114944 ) ) ;
#3371 = EDGE_LOOP ( 'NONE', ( #12735, #6952, #566, #12322, #14100, #14129 ) ) ;
#3372 = CYLINDRICAL_SURFACE ( 'NONE', #14952, 65.24900000006525147 ) ;
#3373 = DIRECTION ( 'NONE',  ( 1.000000000000000000, 0.000000000000000000, 0.000000000000000000 ) ) ;
#3374 = EDGE_CURVE ( 'NONE', #19870, #7692, #14900, .T. ) ;
#3375 = ORIENTED_EDGE ( 'NONE', *, *, #8127, .F. ) ;
#3376 = ORIENTED_EDGE ( 'NONE', *, *, #13097, .T. ) ;
#3377 = CARTESIAN_POINT ( 'NONE',  ( 0.000000000000000000, -67.51707036274397922, -25.00890260772446538 ) ) ;
#3378 = AXIS2_PLACEMENT_3D ( 'NONE', #10016, #5243, #8115 ) ;
#3379 = DIRECTION ( 'NONE',  ( 1.000000000000000000, 0.000000000000000000, 0.000000000000000000 ) ) ;
#3380 = ADVANCED_FACE ( 'NONE', ( #18395 ), #3864, .T. ) ;
#3381 = DIRECTION ( 'NONE',  ( 0.000000000000000000, -1.000000000000000000, 1.287488025362403787E-15 ) ) ;
#3382 = CYLINDRICAL_SURFACE ( 'NONE', #5796, 20.00000000000000000 ) ;
#3383 = CARTESIAN_POINT ( 'NONE',  ( 7.500000000179346316, 1.491842754445843244, 25.19416875018031732 ) ) ;
#3384 = CIRCLE ( 'NONE', #7793, 27.60000000002759535 ) ;
#3385 = CARTESIAN_POINT ( 'NONE',  ( -9.474249097082497073, 6.330490858644137298, 5.540983999713199992 ) ) ;
#3386 = LINE ( 'NONE', #3299, #3538 ) ;
#3387 = LINE ( 'NONE', #11355, #4603 ) ;
#3388 = EDGE_CURVE ( 'NONE', #5518, #8758, #15995, .T. ) ;
#3389 = ORIENTED_EDGE ( 'NONE', *, *, #9192, .F. ) ;
#3390 = CARTESIAN_POINT ( 'NONE',  ( -2.000000000000022649, -3.464101615137742396, -5.600000000000000533 ) ) ;
#3391 = AXIS2_PLACEMENT_3D ( 'NONE', #4599, #6391, #12777 ) ;
#3392 = CARTESIAN_POINT ( 'NONE',  ( 6.888301780572507305, -16.62983158603121936, 15.65073750018031440 ) ) ;
#3393 = DIRECTION ( 'NONE',  ( 0.000000000000000000, 0.000000000000000000, 1.000000000000000000 ) ) ;
#3394 = VERTEX_POINT ( 'NONE', #11822 ) ;
#3395 = EDGE_CURVE ( 'NONE', #18485, #4283, #6941, .T. ) ;
#3396 = DIRECTION ( 'NONE',  ( 0.000000000000000000, 0.000000000000000000, 1.000000000000000000 ) ) ;
#3397 = ORIENTED_EDGE ( 'NONE', *, *, #8433, .T. ) ;
#3398 = DIRECTION ( 'NONE',  ( 0.000000000000000000, 0.000000000000000000, 1.000000000000000000 ) ) ;
#3399 = PLANE ( 'NONE',  #5982 ) ;
#3400 = EDGE_CURVE ( 'NONE', #4144, #11163, #18708, .T. ) ;
#3401 = ORIENTED_EDGE ( 'NONE', *, *, #2147, .T. ) ;
#3402 = ORIENTED_EDGE ( 'NONE', *, *, #13641, .T. ) ;
#3403 = DIRECTION ( 'NONE',  ( 0.000000000000000000, -0.2697967711570313232, 0.9629172873477972461 ) ) ;
#3404 = EDGE_CURVE ( 'NONE', #14263, #1127, #17700, .T. ) ;
#3405 = CARTESIAN_POINT ( 'NONE',  ( 0.000000000000000000, 0.000000000000000000, 0.000000000000000000 ) ) ;
#3406 = CARTESIAN_POINT ( 'NONE',  ( 30.00000000000000000, -99.99999999999998579, 52.00000000000000000 ) ) ;
#3407 = VECTOR ( 'NONE', #16481, 1000.000000000000000 ) ;
#3408 = DIRECTION ( 'NONE',  ( -1.000000000000000000, 0.000000000000000000, 0.000000000000000000 ) ) ;
#3409 = ORIENTED_EDGE ( 'NONE', *, *, #7338, .T. ) ;
#3410 = CARTESIAN_POINT ( 'NONE',  ( -6.358192988180014993, -4.248408729364575365, 4.202706250180310299 ) ) ;
#3411 = FACE_OUTER_BOUND ( 'NONE', #871, .T. ) ;
#3412 = CIRCLE ( 'NONE', #20676, 27.60000000002759890 ) ;
#3413 = CARTESIAN_POINT ( 'NONE',  ( 0.000000000000000000, 59.36728637278019960, 40.73727173906807764 ) ) ;
#3414 = DIRECTION ( 'NONE',  ( 1.000000000000000000, -1.734723475976806848E-16, -0.000000000000000000 ) ) ;
#3415 = ADVANCED_FACE ( 'NONE', ( #2072 ), #13113, .F. ) ;
#3416 = EDGE_LOOP ( 'NONE', ( #3205, #2703, #5913, #2514 ) ) ;
#3417 = CARTESIAN_POINT ( 'NONE',  ( 19.99999999999999645, -38.69327817041812523, 52.53819777490620169 ) ) ;
#3418 = ORIENTED_EDGE ( 'NONE', *, *, #12695, .T. ) ;
#3419 = DIRECTION ( 'NONE',  ( 0.000000000000000000, -0.5195839500354229035, -0.8544194045464950094 ) ) ;
#3420 = CARTESIAN_POINT ( 'NONE',  ( -40.00000000000000000, 29.99999999999999289, -130.0000000000000000 ) ) ;
#3421 = ORIENTED_EDGE ( 'NONE', *, *, #17291, .T. ) ;
#3422 = CARTESIAN_POINT ( 'NONE',  ( -12.50000000000000533, 0.000000000000000000, 43.00000000000000000 ) ) ;
#3423 = ORIENTED_EDGE ( 'NONE', *, *, #5844, .F. ) ;
#3424 = DIRECTION ( 'NONE',  ( 0.000000000000000000, 0.000000000000000000, 1.000000000000000000 ) ) ;
#3425 = ORIENTED_EDGE ( 'NONE', *, *, #3867, .F. ) ;
#3426 = CIRCLE ( 'NONE', #19996, 8.999999999999994671 ) ;
#3427 = AXIS2_PLACEMENT_3D ( 'NONE', #7740, #10717, #18773 ) ;
#3428 = LINE ( 'NONE', #3125, #4328 ) ;
#3429 = ADVANCED_FACE ( 'NONE', ( #6626 ), #6831, .F. ) ;
#3430 = CARTESIAN_POINT ( 'NONE',  ( 6.250000000000054179, 10.82531754730546147, 129.0000000000000000 ) ) ;
#3431 = AXIS2_PLACEMENT_3D ( 'NONE', #4885, #6366, #16015 ) ;
#3432 = CARTESIAN_POINT ( 'NONE',  ( 13.67243654642775574, -5.663308650141541278, -21.37064558115845614 ) ) ;
#3433 = ORIENTED_EDGE ( 'NONE', *, *, #12990, .T. ) ;
#3434 = SURFACE_STYLE_USAGE ( .BOTH. , #16370 ) ;
#3435 = DIRECTION ( 'NONE',  ( 0.000000000000000000, 0.000000000000000000, 1.000000000000000000 ) ) ;
#3436 = VERTEX_POINT ( 'NONE', #10232 ) ;
#3437 = CIRCLE ( 'NONE', #8853, 72.00000000007199219 ) ;
#3438 = CARTESIAN_POINT ( 'NONE',  ( 7.499999999820663454, -1.491842756249032398, -27.60666874981969698 ) ) ;
#3439 = CIRCLE ( 'NONE', #12930, 7.500000000000000000 ) ;
#3440 = EDGE_LOOP ( 'NONE', ( #8664, #8272 ) ) ;
#3441 = CARTESIAN_POINT ( 'NONE',  ( 3.580422614997668340, 17.99999999956958519, 21.24683125018031404 ) ) ;
#3442 = DIRECTION ( 'NONE',  ( -0.000000000000000000, -0.000000000000000000, 1.000000000000000000 ) ) ;
#3443 = CARTESIAN_POINT ( 'NONE',  ( 50.00000000000000000, -139.6410161513775563, -85.00000000000000000 ) ) ;
#3444 = ORIENTED_EDGE ( 'NONE', *, *, #12629, .F. ) ;
#3445 = CARTESIAN_POINT ( 'NONE',  ( 28.13963350654227824, -26.35784117651622793, -120.0000000000000142 ) ) ;
#3446 = ORIENTED_EDGE ( 'NONE', *, *, #33, .T. ) ;
#3447 = CARTESIAN_POINT ( 'NONE',  ( 0.000000000000000000, 0.000000000000000000, -68.00000000000000000 ) ) ;
#3448 = CARTESIAN_POINT ( 'NONE',  ( 9.999999999999998224, 8.857208570070804754, -71.45313048675076573 ) ) ;
#3449 = ORIENTED_EDGE ( 'NONE', *, *, #3404, .F. ) ;
#3450 = DIRECTION ( 'NONE',  ( 0.000000000000000000, 0.000000000000000000, 1.000000000000000000 ) ) ;
#3451 = VECTOR ( 'NONE', #15978, 1000.000000000000000 ) ;
#3452 = CIRCLE ( 'NONE', #16317, 5.000000000000000888 ) ;
#3453 = EDGE_CURVE ( 'NONE', #18447, #15935, #20047, .T. ) ;
#3454 = CARTESIAN_POINT ( 'NONE',  ( -31.75000000000000000, 0.000000000000000000, 0.000000000000000000 ) ) ;
#3455 = CIRCLE ( 'NONE', #5478, 72.00000000007199219 ) ;
#3456 = CARTESIAN_POINT ( 'NONE',  ( -10.19618095047498230, 15.25966317163203279, -8.206293749819689509 ) ) ;
#3457 = ORIENTED_EDGE ( 'NONE', *, *, #16497, .F. ) ;
#3458 = CARTESIAN_POINT ( 'NONE',  ( -4.248408729364577141, 6.358192988180014993, 6.558956250180307812 ) ) ;
#3459 = CARTESIAN_POINT ( 'NONE',  ( 10.46442989202483531, -10.46442989454075168, 1.875333081519072742 ) ) ;
#3460 = CARTESIAN_POINT ( 'NONE',  ( 6.680000000000000604, 6.938893903907228378E-15, 0.000000000000000000 ) ) ;
#3461 = VECTOR ( 'NONE', #15119, 1000.000000000000000 ) ;
#3462 = VECTOR ( 'NONE', #6084, 1000.000000000000000 ) ;
#3463 = ORIENTED_EDGE ( 'NONE', *, *, #3654, .T. ) ;
#3464 = DIRECTION ( 'NONE',  ( 0.000000000000000000, -0.6310879443260593025, 0.7757112907044144690 ) ) ;
#3465 = DIRECTION ( 'NONE',  ( 0.000000000000000000, 1.000000000000000000, 0.000000000000000000 ) ) ;
#3466 = CARTESIAN_POINT ( 'NONE',  ( -24.99999999999999289, 230.0000000000000000, -84.99999999999998579 ) ) ;
#3467 = VERTEX_POINT ( 'NONE', #19566 ) ;
#3468 = CARTESIAN_POINT ( 'NONE',  ( 0.000000000000000000, 0.000000000000000000, 166.0000000000000000 ) ) ;
#3469 = ORIENTED_EDGE ( 'NONE', *, *, #5276, .F. ) ;
#3470 = DIRECTION ( 'NONE',  ( 0.000000000000000000, 0.000000000000000000, 1.000000000000000000 ) ) ;
#3471 = CARTESIAN_POINT ( 'NONE',  ( 0.000000000000000000, 51.43306257653143376, 40.15061736769582268 ) ) ;
#3472 = ORIENTED_EDGE ( 'NONE', *, *, #16669, .F. ) ;
#3473 = ORIENTED_EDGE ( 'NONE', *, *, #15735, .T. ) ;
#3474 = DIRECTION ( 'NONE',  ( 0.000000000000000000, 0.000000000000000000, 1.000000000000000000 ) ) ;
#3475 = CARTESIAN_POINT ( 'NONE',  ( 0.000000000000000000, 0.000000000000000000, -5.600000000000000533 ) ) ;
#3476 = SHAPE_REPRESENTATION_RELATIONSHIP ( 'NONE' , 'NONE' ,  #3036, #7906 ) ;
#3477 = CARTESIAN_POINT ( 'NONE',  ( 6.679999999999997051, 11.50000000000000178, 0.000000000000000000 ) ) ;
#3478 = CIRCLE ( 'NONE', #14661, 5.000000000000004441 ) ;
#3479 = CARTESIAN_POINT ( 'NONE',  ( 19.99999999999999645, 51.81019761368373366, -38.98425606966007706 ) ) ;
#3480 = CARTESIAN_POINT ( 'NONE',  ( -1.491842756249033064, -7.499999999820668783, 9.289481250180317673 ) ) ;
#3481 = EDGE_CURVE ( 'NONE', #14374, #14158, #20407, .T. ) ;
#3482 = CARTESIAN_POINT ( 'NONE',  ( -10.32494394706615815, 4.276731815070940357, -4.178547250286804626 ) ) ;
#3483 = EDGE_CURVE ( 'NONE', #5992, #9439, #11275, .T. ) ;
#3484 = VECTOR ( 'NONE', #15619, 1000.000000000000000 ) ;
#3485 = FACE_OUTER_BOUND ( 'NONE', #2527, .T. ) ;
#3486 = CARTESIAN_POINT ( 'NONE',  ( 2.500000000000000000, 0.000000000000000000, 0.000000000000000000 ) ) ;
#3487 = AXIS2_PLACEMENT_3D ( 'NONE', #18984, #20344, #10922 ) ;
#3488 = ORIENTED_EDGE ( 'NONE', *, *, #17541, .F. ) ;
#3489 = CARTESIAN_POINT ( 'NONE',  ( 1.214306433183764966E-14, 4.618802153517020059, 0.000000000000000000 ) ) ;
#3490 = CARTESIAN_POINT ( 'NONE',  ( -3.580422614997675002, -17.99999999956958163, 16.53433125018031191 ) ) ;
#3491 = DIRECTION ( 'NONE',  ( 1.000000000000000000, 0.000000000000000000, 0.000000000000000000 ) ) ;
#3492 = EDGE_CURVE ( 'NONE', #17770, #14722, #8550, .T. ) ;
#3493 = ORIENTED_EDGE ( 'NONE', *, *, #20509, .T. ) ;
#3494 = AXIS2_PLACEMENT_3D ( 'NONE', #7761, #4472, #20678 ) ;
#3495 = CARTESIAN_POINT ( 'NONE',  ( 19.99999999999999645, 0.000000000000000000, 0.000000000000000000 ) ) ;
#3496 = EDGE_LOOP ( 'NONE', ( #6754, #7783, #1663, #2432 ) ) ;
#3497 = MANIFOLD_SOLID_BREP ( 'Hex', #2199 ) ;
#3498 = DIRECTION ( 'NONE',  ( -1.000000000000000000, -0.000000000000000000, -0.000000000000000000 ) ) ;
#3499 = CARTESIAN_POINT ( 'NONE',  ( 31.36240272394379858, -36.86890566740344610, -66.67347288640101510 ) ) ;
#3500 = EDGE_LOOP ( 'NONE', ( #2727, #10830, #6356, #14645 ) ) ;
#3501 = ORIENTED_EDGE ( 'NONE', *, *, #11043, .F. ) ;
#3502 = CARTESIAN_POINT ( 'NONE',  ( 50.00000000000000000, 36.35083268962915781, 50.00000000000000000 ) ) ;
#3503 = AXIS2_PLACEMENT_3D ( 'NONE', #3622, #456, #6905 ) ;
#3504 = DIRECTION ( 'NONE',  ( -1.000000000000000000, -0.000000000000000000, 0.000000000000000000 ) ) ;
#3505 = AXIS2_PLACEMENT_3D ( 'NONE', #6432, #8235, #19577 ) ;
#3506 = ADVANCED_FACE ( 'NONE', ( #5669 ), #13425, .T. ) ;
#3507 = CARTESIAN_POINT ( 'NONE',  ( 3.999999999999990674, -2.309401076758548221, -5.242734410091827613 ) ) ;
#3508 = VECTOR ( 'NONE', #2241, 1000.000000000000000 ) ;
#3509 = ORIENTED_EDGE ( 'NONE', *, *, #20613, .F. ) ;
#3510 = EDGE_CURVE ( 'NONE', #11331, #13140, #5162, .T. ) ;
#3511 = CARTESIAN_POINT ( 'NONE',  ( 5.303300859536630441, 5.303300858261584594, 18.04567500018031367 ) ) ;
#3512 = ADVANCED_FACE ( 'NONE', ( #15319 ), #806, .T. ) ;
#3513 = CARTESIAN_POINT ( 'NONE',  ( 36.57435087158915366, -119.8477454916768181, -84.70193698065399701 ) ) ;
#3514 = PLANE ( 'NONE',  #18968 ) ;
#3515 = DIRECTION ( 'NONE',  ( 0.000000000000000000, 0.000000000000000000, -1.000000000000000000 ) ) ;
#3516 = CARTESIAN_POINT ( 'NONE',  ( 29.74873734152916782, 24.74873734152916072, -120.0000000000000142 ) ) ;
#3517 = ORIENTED_EDGE ( 'NONE', *, *, #18343, .T. ) ;
#3518 = CARTESIAN_POINT ( 'NONE',  ( -6.358192987158597376, 4.248408730893249441, 2.809793750180315186 ) ) ;
#3519 = VERTEX_POINT ( 'NONE', #17014 ) ;
#3520 = ADVANCED_FACE ( 'NONE', ( #18608 ), #7254, .F. ) ;
#3521 = LINE ( 'NONE', #9788, #2249 ) ;
#3522 = CARTESIAN_POINT ( 'NONE',  ( 9.999999999999998224, -59.36728637278047671, 40.73727173906767973 ) ) ;
#3523 = AXIS2_PLACEMENT_3D ( 'NONE', #10846, #7984, #9364 ) ;
#3524 = ORIENTED_EDGE ( 'NONE', *, *, #13526, .F. ) ;
#3525 = CARTESIAN_POINT ( 'NONE',  ( -6.359999999999997655, 4.663913298532544267E-15, 0.000000000000000000 ) ) ;
#3526 = VERTEX_POINT ( 'NONE', #2501 ) ;
#3527 = DIRECTION ( 'NONE',  ( 1.000000000000000000, -0.000000000000000000, -0.000000000000000000 ) ) ;
#3528 = CARTESIAN_POINT ( 'NONE',  ( -52.00000000000000000, -99.99999999999998579, 5.000000000000000000 ) ) ;
#3529 = VERTEX_POINT ( 'NONE', #18506 ) ;
#3530 = AXIS2_PLACEMENT_3D ( 'NONE', #20236, #10173, #5604 ) ;
#3531 = EDGE_CURVE ( 'NONE', #17620, #254, #19726, .T. ) ;
#3532 = CARTESIAN_POINT ( 'NONE',  ( 0.000000000000000000, -51.96384592647165590, -49.83732252579670075 ) ) ;
#3533 = EDGE_CURVE ( 'NONE', #17222, #9460, #9582, .T. ) ;
#3534 = CARTESIAN_POINT ( 'NONE',  ( 19.99999999999999645, 63.05226888949912478, -15.11556105343395906 ) ) ;
#3535 = AXIS2_PLACEMENT_3D ( 'NONE', #14090, #1374, #14512 ) ;
#3536 = CARTESIAN_POINT ( 'NONE',  ( 9.474249098604511587, 6.330490856366296271, 6.184016000647427624 ) ) ;
#3537 = ORIENTED_EDGE ( 'NONE', *, *, #10477, .F. ) ;
#3538 = VECTOR ( 'NONE', #6460, 1000.000000000000000 ) ;
#3539 = EDGE_CURVE ( 'NONE', #10636, #13652, #17953, .T. ) ;
#3540 = LINE ( 'NONE', #16682, #18987 ) ;
#3541 = EDGE_LOOP ( 'NONE', ( #20306, #18788, #20233, #635 ) ) ;
#3542 = CARTESIAN_POINT ( 'NONE',  ( 10.00000000000000178, -160.0000000000000000, -66.80000000000001137 ) ) ;
#3543 = AXIS2_PLACEMENT_3D ( 'NONE', #6870, #20115, #11759 ) ;
#3544 = VERTEX_POINT ( 'NONE', #340 ) ;
#3545 = CARTESIAN_POINT ( 'NONE',  ( 21.00000000000000355, 2.789133085058097101E-16, -2.055000000000000160 ) ) ;
#3546 = CYLINDRICAL_SURFACE ( 'NONE', #12052, 27.60000000002759535 ) ;
#3547 = FACE_OUTER_BOUND ( 'NONE', #5763, .T. ) ;
#3548 = ORIENTED_EDGE ( 'NONE', *, *, #15150, .T. ) ;
#3549 = CARTESIAN_POINT ( 'NONE',  ( 0.000000000000000000, 0.000000000000000000, 43.00000000000000000 ) ) ;
#3550 = PRODUCT_DEFINITION_FORMATION_WITH_SPECIFIED_SOURCE ( 'ANY', '', #18644, .NOT_KNOWN. ) ;
#3551 = EDGE_LOOP ( 'NONE', ( #3644, #9218, #121, #10134 ) ) ;
#3552 =( NAMED_UNIT ( * ) SI_UNIT ( $, .STERADIAN. ) SOLID_ANGLE_UNIT ( ) );
#3553 = CARTESIAN_POINT ( 'NONE',  ( 19.99999999999999645, 63.48283426024897835, -33.96954156735303343 ) ) ;
#3554 = APPLICATION_CONTEXT ( 'automotive_design' ) ;
#3555 = ORIENTED_EDGE ( 'NONE', *, *, #17909, .F. ) ;
#3556 = CARTESIAN_POINT ( 'NONE',  ( 2.870125741905214412, -6.929096494179682431, -10.44411249981968481 ) ) ;
#3557 = PRODUCT_DEFINITION_SHAPE ( 'NONE', 'NONE',  #2358 ) ;
#3558 = FACE_OUTER_BOUND ( 'NONE', #17089, .T. ) ;
#3559 = APPLICATION_PROTOCOL_DEFINITION ( 'draft international standard', 'automotive_design', 1998, #2486 ) ;
#3560 = CARTESIAN_POINT ( 'NONE',  ( -2.943691925285397470, 14.79893867793684059, 13.08951066884154635 ) ) ;
#3561 = ORIENTED_EDGE ( 'NONE', *, *, #5172, .T. ) ;
#3562 = DIRECTION ( 'NONE',  ( -1.000000000000000000, 0.000000000000000000, -0.000000000000000000 ) ) ;
#3563 = DIRECTION ( 'NONE',  ( 0.000000000000000000, 0.000000000000000000, 1.000000000000000000 ) ) ;
#3564 = CARTESIAN_POINT ( 'NONE',  ( -5.663308650141535949, -13.67243654642774686, -5.782479418480926725 ) ) ;
#3565 = MANIFOLD_SOLID_BREP ( 'M6 Clearance Hole1', #17696 ) ;
#3566 = AXIS2_PLACEMENT_3D ( 'NONE', #5910, #12381, #18849 ) ;
#3567 = CARTESIAN_POINT ( 'NONE',  ( 30.00000000000000000, -85.00000000000000000, -1.040949779275250179E-14 ) ) ;
#3568 = EDGE_CURVE ( 'NONE', #2187, #13609, #558, .T. ) ;
#3569 = CIRCLE ( 'NONE', #14097, 27.60000000002759535 ) ;
#3570 = ORIENTED_EDGE ( 'NONE', *, *, #18438, .F. ) ;
#3571 = EDGE_CURVE ( 'NONE', #16945, #11468, #11856, .T. ) ;
#3572 = CARTESIAN_POINT ( 'NONE',  ( 9.999999999999998224, 18.50424539729942808, -69.58155576219097327 ) ) ;
#3573 = CARTESIAN_POINT ( 'NONE',  ( 9.015937996181835182E-10, 7.500000000000002665, 16.86755000018030870 ) ) ;
#3574 = ORIENTED_EDGE ( 'NONE', *, *, #5563, .F. ) ;
#3575 = CARTESIAN_POINT ( 'NONE',  ( 150.0000507999999968, 5.400000000000000355, 1.000000000000000000 ) ) ;
#3576 = ORIENTED_EDGE ( 'NONE', *, *, #16490, .F. ) ;
#3577 = PLANE ( 'NONE',  #20013 ) ;
#3578 = DIRECTION ( 'NONE',  ( 1.000000000000000000, 0.000000000000000000, 0.000000000000000000 ) ) ;
#3579 = ORIENTED_EDGE ( 'NONE', *, *, #19224, .F. ) ;
#3580 = EDGE_LOOP ( 'NONE', ( #20126, #10307, #18630, #17660 ) ) ;
#3581 = CARTESIAN_POINT ( 'NONE',  ( 7.500000000000007105, 4.207617034055637320E-15, 6.638700000002313750 ) ) ;
#3582 = COLOUR_RGB ( '', 0.09019608, 0.27058824, 0.51372549) ;
#3583 = VECTOR ( 'NONE', #4127, 1000.000000000000000 ) ;
#3584 = CARTESIAN_POINT ( 'NONE',  ( 0.000000000000000000, 0.000000000000000000, -7.500000000000000000 ) ) ;
#3585 = DIRECTION ( 'NONE',  ( 1.000000000000000000, 0.000000000000000000, 0.000000000000000000 ) ) ;
#3586 = CARTESIAN_POINT ( 'NONE',  ( 2.500000000000000000, 2.357898499370431722, -2.818925648462311528E-15 ) ) ;
#3587 = CIRCLE ( 'NONE', #18539, 27.60000000002759890 ) ;
#3588 = TOROIDAL_SURFACE ( 'NONE', #8671, 7.567219999999999835, 0.06721999999999891950 ) ;
#3589 = DIRECTION ( 'NONE',  ( -0.000000000000000000, -0.000000000000000000, -1.000000000000000000 ) ) ;
#3590 = CARTESIAN_POINT ( 'NONE',  ( -2.870125741905213079, 6.929096494179683319, 13.11838750018031519 ) ) ;
#3591 = CARTESIAN_POINT ( 'NONE',  ( -10.32494394706615815, 4.276731815070940357, 5.246452749713198749 ) ) ;
#3592 = CIRCLE ( 'NONE', #15799, 79.99999999999997158 ) ;
#3593 = CYLINDRICAL_SURFACE ( 'NONE', #7695, 65.24900000006525147 ) ;
#3594 = DIRECTION ( 'NONE',  ( 1.000000000000000000, 0.000000000000000000, 0.000000000000000000 ) ) ;
#3595 = VECTOR ( 'NONE', #9362, 1000.000000000000000 ) ;
#3596 = VERTEX_POINT ( 'NONE', #6698 ) ;
#3597 = ADVANCED_FACE ( 'NONE', ( #19733 ), #3514, .T. ) ;
#3598 = CARTESIAN_POINT ( 'NONE',  ( 62.50000000000000000, -120.0000000000000142, 0.000000000000000000 ) ) ;
#3599 = AXIS2_PLACEMENT_3D ( 'NONE', #16413, #3182, #2006 ) ;
#3600 = CARTESIAN_POINT ( 'NONE',  ( 10.19618095414378800, 15.25966316918061416, 12.41089375018031227 ) ) ;
#3601 = CYLINDRICAL_SURFACE ( 'NONE', #15132, 65.24900000006525147 ) ;
#3602 = ORIENTED_EDGE ( 'NONE', *, *, #388, .T. ) ;
#3603 = CARTESIAN_POINT ( 'NONE',  ( 30.00000000000000000, -49.99999999999999289, -71.93747284969079203 ) ) ;
#3604 = VERTEX_POINT ( 'NONE', #19932 ) ;
#3605 = FACE_OUTER_BOUND ( 'NONE', #2598, .T. ) ;
#3606 = LINE ( 'NONE', #16432, #20536 ) ;
#3607 = ORIENTED_EDGE ( 'NONE', *, *, #6706, .F. ) ;
#3608 = VERTEX_POINT ( 'NONE', #11680 ) ;
#3609 = DIRECTION ( 'NONE',  ( 0.000000000000000000, 0.000000000000000000, -1.000000000000000000 ) ) ;
#3610 = EDGE_CURVE ( 'NONE', #18776, #10147, #14581, .T. ) ;
#3611 = CIRCLE ( 'NONE', #17532, 2.500000000000000888 ) ;
#3612 = LINE ( 'NONE', #335, #7941 ) ;
#3613 = CIRCLE ( 'NONE', #9389, 8.500000000000000000 ) ;
#3614 = DIRECTION ( 'NONE',  ( -1.000000000000000000, 0.000000000000000000, -0.000000000000000000 ) ) ;
#3615 = ADVANCED_FACE ( 'NONE', ( #11881 ), #453, .T. ) ;
#3616 = CIRCLE ( 'NONE', #581, 10.85999999999999233 ) ;
#3617 = CARTESIAN_POINT ( 'NONE',  ( -6.358192987158591158, 4.248408730893245000, 15.39489375018031403 ) ) ;
#3618 = CIRCLE ( 'NONE', #11410, 11.50000000000000000 ) ;
#3619 = CARTESIAN_POINT ( 'NONE',  ( -25.00000000000000000, -30.00000000000000711, -58.09475019311124555 ) ) ;
#3620 = FACE_OUTER_BOUND ( 'NONE', #9347, .T. ) ;
#3621 = DIRECTION ( 'NONE',  ( -1.000000000000000000, 0.000000000000000000, 0.000000000000000000 ) ) ;
#3622 = CARTESIAN_POINT ( 'NONE',  ( 52.00000000000000000, -39.99999999999999289, 5.000000000000000000 ) ) ;
#3623 = VERTEX_POINT ( 'NONE', #5410 ) ;
#3624 = DIRECTION ( 'NONE',  ( 0.000000000000000000, 0.000000000000000000, 1.000000000000000000 ) ) ;
#3625 = ORIENTED_EDGE ( 'NONE', *, *, #16188, .F. ) ;
#3626 = CARTESIAN_POINT ( 'NONE',  ( 18.13963350654227469, -26.35784117651622793, -120.0000000000000142 ) ) ;
#3627 = CARTESIAN_POINT ( 'NONE',  ( 19.99999999999999645, 54.08351995568706627, 35.76369202524519864 ) ) ;
#3628 = VERTEX_POINT ( 'NONE', #5103 ) ;
#3629 = PLANE ( 'NONE',  #9594 ) ;
#3630 = ORIENTED_EDGE ( 'NONE', *, *, #13538, .T. ) ;
#3631 = LINE ( 'NONE', #19849, #6436 ) ;
#3632 = DIRECTION ( 'NONE',  ( -2.249565377136137858E-32, 1.224646799147353207E-16, 1.000000000000000000 ) ) ;
#3633 = AXIS2_PLACEMENT_3D ( 'NONE', #20403, #4400, #7791 ) ;
#3634 = VERTEX_POINT ( 'NONE', #15176 ) ;
#3635 = EDGE_CURVE ( 'NONE', #13015, #1598, #13898, .T. ) ;
#3636 = EDGE_CURVE ( 'NONE', #12585, #7176, #2042, .T. ) ;
#3637 = CYLINDRICAL_SURFACE ( 'NONE', #18891, 2.099999999999997868 ) ;
#3638 = CARTESIAN_POINT ( 'NONE',  ( 0.000000000000000000, -31.17893654894269773, 57.31758819669160232 ) ) ;
#3639 = ADVANCED_FACE ( 'NONE', ( #16872 ), #13277, .T. ) ;
#3640 = DIRECTION ( 'NONE',  ( 1.000000000000000000, 0.000000000000000000, 0.000000000000000000 ) ) ;
#3641 = ADVANCED_FACE ( 'NONE', ( #3620 ), #10852, .T. ) ;
#3642 = CARTESIAN_POINT ( 'NONE',  ( 4.276731812588570492, -10.32494394809439697, 8.834797250647429934 ) ) ;
#3643 = PRODUCT_RELATED_PRODUCT_CATEGORY ( 'part', '', ( #5599 ) ) ;
#3644 = ORIENTED_EDGE ( 'NONE', *, *, #8540, .T. ) ;
#3645 =( LENGTH_UNIT ( ) NAMED_UNIT ( * ) SI_UNIT ( .MILLI., .METRE. ) );
#3646 = FACE_OUTER_BOUND ( 'NONE', #6621, .T. ) ;
#3647 = VERTEX_POINT ( 'NONE', #18352 ) ;
#3648 = DIRECTION ( 'NONE',  ( 1.000000000000000000, 1.836909530733573776E-16, 0.000000000000000000 ) ) ;
#3649 = VERTEX_POINT ( 'NONE', #10093 ) ;
#3650 = CARTESIAN_POINT ( 'NONE',  ( 10.19618095414378800, 15.25966316918061416, 12.41089375018031227 ) ) ;
#3651 = DIRECTION ( 'NONE',  ( 1.000000000000000000, 1.836909530733573776E-16, 0.000000000000000000 ) ) ;
#3652 = DIRECTION ( 'NONE',  ( 0.000000000000000000, 0.000000000000000000, -1.000000000000000000 ) ) ;
#3653 = EDGE_CURVE ( 'NONE', #1772, #19446, #7111, .T. ) ;
#3654 = EDGE_CURVE ( 'NONE', #8524, #8783, #15987, .T. ) ;
#3655 = ORIENTED_EDGE ( 'NONE', *, *, #9080, .F. ) ;
#3656 = ADVANCED_BREP_SHAPE_REPRESENTATION ( '', ( #3565, #12461 ), #2940 ) ;
#3657 = CYLINDRICAL_SURFACE ( 'NONE', #15141, 10.00000000000000178 ) ;
#3658 = ORIENTED_EDGE ( 'NONE', *, *, #1134, .F. ) ;
#3659 = CARTESIAN_POINT ( 'NONE',  ( 30.00000000000000000, -30.00000000000000711, 50.99019513592783426 ) ) ;
#3660 = EDGE_CURVE ( 'NONE', #15594, #6600, #17381, .T. ) ;
#3661 = VERTEX_POINT ( 'NONE', #12105 ) ;
#3662 = CARTESIAN_POINT ( 'NONE',  ( 0.000000000000000000, 0.000000000000000000, -84.99999999999998579 ) ) ;
#3663 = ADVANCED_FACE ( 'NONE', ( #9521 ), #9815, .T. ) ;
#3664 = CARTESIAN_POINT ( 'NONE',  ( 0.000000000000000000, -6.872116855663586321, 64.47358224882414390 ) ) ;
#3665 = PRODUCT_CONTEXT ( 'NONE', #18324, 'mechanical' ) ;
#3666 = CARTESIAN_POINT ( 'NONE',  ( 14.79893867793684059, 2.943691925285398359, 24.87076066884155168 ) ) ;
#3667 = ORIENTED_EDGE ( 'NONE', *, *, #12868, .T. ) ;
#3668 = LINE ( 'NONE', #11734, #5496 ) ;
#3669 = FACE_OUTER_BOUND ( 'NONE', #874, .T. ) ;
#3670 = CARTESIAN_POINT ( 'NONE',  ( 13.67243654642774686, -5.663308650141536837, -26.98872941848093276 ) ) ;
#3671 = PLANE ( 'NONE',  #422 ) ;
#3672 = AXIS2_PLACEMENT_3D ( 'NONE', #19102, #15907, #14224 ) ;
#3673 = EDGE_CURVE ( 'NONE', #19655, #16611, #1491, .T. ) ;
#3674 = ORIENTED_EDGE ( 'NONE', *, *, #10485, .T. ) ;
#3675 = CARTESIAN_POINT ( 'NONE',  ( 34.81051331576767183, -118.0383536556227995, 83.29664741859293997 ) ) ;
#3676 = LINE ( 'NONE', #19679, #1283 ) ;
#3677 = ORIENTED_EDGE ( 'NONE', *, *, #3770, .T. ) ;
#3678 = CARTESIAN_POINT ( 'NONE',  ( 19.99999999999999645, -63.05226888949880504, -15.11556105343524514 ) ) ;
#3679 = ORIENTED_EDGE ( 'NONE', *, *, #17282, .T. ) ;
#3680 = CARTESIAN_POINT ( 'NONE',  ( 19.99999999999999645, 27.62776854598936538, -58.65812137498974721 ) ) ;
#3681 = CARTESIAN_POINT ( 'NONE',  ( 10.19618095414378622, 15.25966316918061239, 10.50629375018031020 ) ) ;
#3682 = VERTEX_POINT ( 'NONE', #3059 ) ;
#3683 = ORIENTED_EDGE ( 'NONE', *, *, #17475, .F. ) ;
#3684 = DIRECTION ( 'NONE',  ( -0.000000000000000000, -0.000000000000000000, -1.000000000000000000 ) ) ;
#3685 = DIRECTION ( 'NONE',  ( 1.000000000000000000, 0.000000000000000000, 0.000000000000000000 ) ) ;
#3686 = CARTESIAN_POINT ( 'NONE',  ( 0.000000000000000000, -59.31169354540756444, 27.19476070466835438 ) ) ;
#3687 =( NAMED_UNIT ( * ) PLANE_ANGLE_UNIT ( ) SI_UNIT ( $, .RADIAN. ) );
#3688 = CARTESIAN_POINT ( 'NONE',  ( 6.888301780572508193, -16.62983158603122291, 15.65073750018031262 ) ) ;
#3689 = UNCERTAINTY_MEASURE_WITH_UNIT (LENGTH_MEASURE( 1.000000000000000082E-05 ), #10185, 'distance_accuracy_value', 'NONE');
#3690 = EDGE_CURVE ( 'NONE', #12734, #15337, #16967, .T. ) ;
#3691 = CARTESIAN_POINT ( 'NONE',  ( 0.000000000000000000, 18.50424539729942808, -69.58155576219097327 ) ) ;
#3692 = CARTESIAN_POINT ( 'NONE',  ( -4.248408730893249441, -6.358192987158595599, -8.971456249819688367 ) ) ;
#3693 = CARTESIAN_POINT ( 'NONE',  ( -2.222972771497743416, -11.17563879704981566, -16.25432850028680676 ) ) ;
#3694 = CARTESIAN_POINT ( 'NONE',  ( -26.35784117651625280, 26.35784117651607872, -130.0000000000000000 ) ) ;
#3695 = CARTESIAN_POINT ( 'NONE',  ( 2.000000000000010658, -3.464101615137748169, -5.600000000000000533 ) ) ;
#3696 = ORIENTED_EDGE ( 'NONE', *, *, #10532, .T. ) ;
#3697 = CARTESIAN_POINT ( 'NONE',  ( -24.99999999999999289, -159.9999999999999716, -85.00000000000000000 ) ) ;
#3698 = CARTESIAN_POINT ( 'NONE',  ( -6.888301780572501976, 16.62983158603122291, 1.513237500180310890 ) ) ;
#3699 = CARTESIAN_POINT ( 'NONE',  ( 0.000000000000000000, 0.000000000000000000, 0.000000000000000000 ) ) ;
#3700 = ORIENTED_EDGE ( 'NONE', *, *, #13988, .F. ) ;
#3701 = DIRECTION ( 'NONE',  ( 0.000000000000000000, -1.000000000000000000, 1.287488025362403787E-15 ) ) ;
#3702 = CIRCLE ( 'NONE', #15898, 72.00000000007199219 ) ;
#3703 = ORIENTED_EDGE ( 'NONE', *, *, #14681, .T. ) ;
#3704 = FACE_OUTER_BOUND ( 'NONE', #10097, .T. ) ;
#3705 = CARTESIAN_POINT ( 'NONE',  ( 19.99999999999999645, 0.000000000000000000, 0.000000000000000000 ) ) ;
#3706 = ORIENTED_EDGE ( 'NONE', *, *, #9777, .T. ) ;
#3707 = ORIENTED_EDGE ( 'NONE', *, *, #18942, .T. ) ;
#3708 = CYLINDRICAL_SURFACE ( 'NONE', #19167, 27.60000000002759890 ) ;
#3709 = DIRECTION ( 'NONE',  ( -1.000000000000000000, -0.000000000000000000, -0.000000000000000000 ) ) ;
#3710 = EDGE_CURVE ( 'NONE', #20532, #3970, #15385, .T. ) ;
#3711 = CARTESIAN_POINT ( 'NONE',  ( -52.00000000000000000, -99.99999999999998579, 5.000000000000000000 ) ) ;
#3712 = CARTESIAN_POINT ( 'NONE',  ( -6.929096494179677101, -2.870125741905209527, 13.92223750018031225 ) ) ;
#3713 = AXIS2_PLACEMENT_3D ( 'NONE', #5653, #20598, #18810 ) ;
#3714 = CARTESIAN_POINT ( 'NONE',  ( 31.32223236346404960, -112.1651446957970819, -79.86480430250811935 ) ) ;
#3715 = CARTESIAN_POINT ( 'NONE',  ( 4.000000000000003553, 0.3904826640788068293, -5.599999999999999645 ) ) ;
#3716 = CARTESIAN_POINT ( 'NONE',  ( -4.000000000000000000, -1.549102112939103826, -0.1578953385959410982 ) ) ;
#3717 = VERTEX_POINT ( 'NONE', #13807 ) ;
#3718 = CARTESIAN_POINT ( 'NONE',  ( 17.50000000000000355, 2.143131898507868643E-15, 46.00000000000000711 ) ) ;
#3719 = ORIENTED_EDGE ( 'NONE', *, *, #2752, .F. ) ;
#3720 = CARTESIAN_POINT ( 'NONE',  ( -6.888301784570738384, -16.62983158437509346, -3.925737499819687670 ) ) ;
#3721 = DIRECTION ( 'NONE',  ( 0.000000000000000000, 0.000000000000000000, 1.000000000000000000 ) ) ;
#3722 = CIRCLE ( 'NONE', #15583, 27.60000000002760601 ) ;
#3723 = ORIENTED_EDGE ( 'NONE', *, *, #12491, .T. ) ;
#3724 = CYLINDRICAL_SURFACE ( 'NONE', #106, 10.00000000000000178 ) ;
#3725 = ORIENTED_EDGE ( 'NONE', *, *, #18967, .T. ) ;
#3726 = PRODUCT_DEFINITION_SHAPE ( 'NONE', 'NONE',  #20965 ) ;
#3727 = CARTESIAN_POINT ( 'NONE',  ( 19.99999999999999645, -1.971042061628798470, 64.80882494896106039 ) ) ;
#3728 = LINE ( 'NONE', #4157, #20519 ) ;
#3729 = ORIENTED_EDGE ( 'NONE', *, *, #8582, .T. ) ;
#3730 = AXIS2_PLACEMENT_3D ( 'NONE', #13514, #8414, #7237 ) ;
#3731 = FACE_BOUND ( 'NONE', #5116, .T. ) ;
#3732 = CARTESIAN_POINT ( 'NONE',  ( -16.62983158603121936, -6.888301780572499311, -2.747612499819688914 ) ) ;
#3733 = VECTOR ( 'NONE', #5318, 1000.000000000000000 ) ;
#3734 = CARTESIAN_POINT ( 'NONE',  ( -23.00000000000000000, 2.816687638038912352E-15, -90.00000000000000000 ) ) ;
#3735 = CARTESIAN_POINT ( 'NONE',  ( 6.330490858644141738, 9.474249097082498849, 5.594953500647431355 ) ) ;
#3736 = ORIENTED_EDGE ( 'NONE', *, *, #14493, .F. ) ;
#3737 = FILL_AREA_STYLE_COLOUR ( '', #10997 ) ;
#3738 = DIRECTION ( 'NONE',  ( -1.000000000000000000, 0.000000000000000000, 0.000000000000000000 ) ) ;
#3739 = ORIENTED_EDGE ( 'NONE', *, *, #13222, .T. ) ;
#3740 = CARTESIAN_POINT ( 'NONE',  ( 10.47959250967882738, -18.77674085041570606, -71.79709706900058563 ) ) ;
#3741 = ADVANCED_FACE ( 'NONE', ( #12608 ), #15885, .F. ) ;
#3742 = ORIENTED_EDGE ( 'NONE', *, *, #150, .F. ) ;
#3743 = EDGE_CURVE ( 'NONE', #6167, #19712, #12539, .T. ) ;
#3744 = CARTESIAN_POINT ( 'NONE',  ( 2.163825119083639534E-09, 18.00000000000000000, 11.52730000018031298 ) ) ;
#3745 = CYLINDRICAL_SURFACE ( 'NONE', #4945, 5.000000000000004441 ) ;
#3746 = CARTESIAN_POINT ( 'NONE',  ( 19.99999999999999645, -18.50424539729892359, 69.58155576219108696 ) ) ;
#3747 = EDGE_LOOP ( 'NONE', ( #14466, #12028, #9213, #18114, #14899, #13729, #2630 ) ) ;
#3748 = DIRECTION ( 'NONE',  ( -1.000000000000000000, 0.000000000000000000, 0.000000000000000000 ) ) ;
#3749 = CIRCLE ( 'NONE', #7822, 27.60000000002759890 ) ;
#3750 = ADVANCED_FACE ( 'NONE', ( #14307 ), #5624, .T. ) ;
#3751 = ORIENTED_EDGE ( 'NONE', *, *, #1690, .T. ) ;
#3752 = CARTESIAN_POINT ( 'NONE',  ( 19.99999999999999645, 1.971042061628357933, 64.80882494896107460 ) ) ;
#3753 = ORIENTED_EDGE ( 'NONE', *, *, #12180, .F. ) ;
#3754 = CARTESIAN_POINT ( 'NONE',  ( 17.99999999999999645, -2.163824016901520184E-09, -25.72104999981969442 ) ) ;
#3755 = DIRECTION ( 'NONE',  ( -1.000000000000000000, -0.000000000000000000, 0.000000000000000000 ) ) ;
#3756 = ITEM_DEFINED_TRANSFORMATION ( 'NONE', 'NONE', #11039,  #12461 ) ;
#3757 = CARTESIAN_POINT ( 'NONE',  ( -12.54593441562641054, 8.382925371439629458, 21.33638566884155097 ) ) ;
#3758 = VECTOR ( 'NONE', #15586, 1000.000000000000000 ) ;
#3759 = ADVANCED_FACE ( 'NONE', ( #5725 ), #868, .T. ) ;
#3760 = ORIENTED_EDGE ( 'NONE', *, *, #20339, .F. ) ;
#3761 = DIRECTION ( 'NONE',  ( -1.000000000000000000, 0.000000000000000000, 0.000000000000000000 ) ) ;
#3762 = CONICAL_SURFACE ( 'NONE', #5460, 4.000000000000000000, 1.047197551196595855 ) ;
#3763 = ORIENTED_EDGE ( 'NONE', *, *, #18343, .F. ) ;
#3764 = FACE_OUTER_BOUND ( 'NONE', #7305, .T. ) ;
#3765 = ADVANCED_FACE ( 'NONE', ( #13904 ), #7321, .T. ) ;
#3766 = CARTESIAN_POINT ( 'NONE',  ( 1.779017513685135741E-09, 14.79893867758296544, -20.50904191848093205 ) ) ;
#3767 = EDGE_CURVE ( 'NONE', #141, #5576, #19633, .T. ) ;
#3768 = CARTESIAN_POINT ( 'NONE',  ( 6.250000000000054179, 10.82531754730546147, 169.0000000000000000 ) ) ;
#3769 = ORIENTED_EDGE ( 'NONE', *, *, #18633, .T. ) ;
#3770 = EDGE_CURVE ( 'NONE', #7037, #4233, #3384, .T. ) ;
#3771 = CARTESIAN_POINT ( 'NONE',  ( 34.02361417125685250, -117.0388906796276700, 82.60709736717031149 ) ) ;
#3772 = CARTESIAN_POINT ( 'NONE',  ( 50.00000000000000000, -139.6410161513775563, 85.00000000000000000 ) ) ;
#3773 = EDGE_LOOP ( 'NONE', ( #1695, #19820 ) ) ;
#3774 = AXIS2_PLACEMENT_3D ( 'NONE', #2609, #7140, #17010 ) ;
#3775 = CARTESIAN_POINT ( 'NONE',  ( -6.358192988180021210, -4.248408729364580694, 10.46760625018031554 ) ) ;
#3776 = VECTOR ( 'NONE', #16946, 1000.000000000000000 ) ;
#3777 = ORIENTED_EDGE ( 'NONE', *, *, #14687, .F. ) ;
#3778 = DIRECTION ( 'NONE',  ( -1.000000000000000000, 0.000000000000000000, 0.000000000000000000 ) ) ;
#3779 = CARTESIAN_POINT ( 'NONE',  ( 17.99999999999999645, -2.163824016901520184E-09, 11.97895000018031020 ) ) ;
#3780 = ORIENTED_EDGE ( 'NONE', *, *, #433, .T. ) ;
#3781 = CIRCLE ( 'NONE', #16652, 0.3200000000000008393 ) ;
#3782 = ORIENTED_EDGE ( 'NONE', *, *, #18434, .F. ) ;
#3783 = CARTESIAN_POINT ( 'NONE',  ( -21.35784117651625280, 26.35784117651607872, -130.0000000000000000 ) ) ;
#3784 = FACE_OUTER_BOUND ( 'NONE', #18898, .T. ) ;
#3785 = CARTESIAN_POINT ( 'NONE',  ( 19.99999999999999645, 63.05226888949891162, 15.11556105343481882 ) ) ;
#3786 = SURFACE_SIDE_STYLE ('',( #1051 ) ) ;
#3787 = CARTESIAN_POINT ( 'NONE',  ( 18.00000000043041481, 3.580422610670020322, 23.01401875018030907 ) ) ;
#3788 = ADVANCED_FACE ( 'NONE', ( #14414 ), #17487, .T. ) ;
#3789 = CYLINDRICAL_SURFACE ( 'NONE', #3543, 2.649999999999994582 ) ;
#3790 = CARTESIAN_POINT ( 'NONE',  ( -7.499999999820669672, 1.491842756249032620, -7.204268749819685347 ) ) ;
#3791 = AXIS2_PLACEMENT_3D ( 'NONE', #8035, #11210, #11113 ) ;
#3792 = AXIS2_PLACEMENT_3D ( 'NONE', #10664, #4293, #17334 ) ;
#3793 = CARTESIAN_POINT ( 'NONE',  ( 11.17563879704981566, -2.222972771497744304, -18.61057850028680605 ) ) ;
#3794 = EDGE_CURVE ( 'NONE', #9645, #14918, #4656, .T. ) ;
#3795 = LINE ( 'NONE', #846, #6006 ) ;
#3796 = DIRECTION ( 'NONE',  ( 1.000000000000000000, 0.000000000000000000, 0.000000000000000000 ) ) ;
#3797 = ORIENTED_EDGE ( 'NONE', *, *, #11190, .F. ) ;
#3798 = PLANE ( 'NONE',  #7870 ) ;
#3799 = CARTESIAN_POINT ( 'NONE',  ( 18.00000000000000000, -2.163824016901520184E-09, 4.458550000180312445 ) ) ;
#3800 = CARTESIAN_POINT ( 'NONE',  ( 0.000000000000000000, 0.000000000000000000, -130.0000000000000000 ) ) ;
#3801 = AXIS2_PLACEMENT_3D ( 'NONE', #14069, #6095, #2620 ) ;
#3802 = VERTEX_POINT ( 'NONE', #759 ) ;
#3803 = CARTESIAN_POINT ( 'NONE',  ( -30.00000000000000000, -164.9999999999999716, 90.00000000000001421 ) ) ;
#3804 = ORIENTED_EDGE ( 'NONE', *, *, #3653, .F. ) ;
#3805 = CARTESIAN_POINT ( 'NONE',  ( -6.165580000000000283, 0.000000000000000000, 0.000000000000000000 ) ) ;
#3806 = ADVANCED_FACE ( 'NONE', ( #13694 ), #16259, .T. ) ;
#3807 = ORIENTED_EDGE ( 'NONE', *, *, #5704, .F. ) ;
#3808 = ORIENTED_EDGE ( 'NONE', *, *, #14738, .F. ) ;
#3809 = CARTESIAN_POINT ( 'NONE',  ( 50.00000000000000000, 36.35083268962920044, -90.00000000000000000 ) ) ;
#3810 = CONICAL_SURFACE ( 'NONE', #6181, 2.041999999999999815, 1.047197551196591858 ) ;
#3811 =( NAMED_UNIT ( * ) PLANE_ANGLE_UNIT ( ) SI_UNIT ( $, .RADIAN. ) );
#3812 = CYLINDRICAL_SURFACE ( 'NONE', #15681, 27.60000000002760245 ) ;
#3813 = FACE_OUTER_BOUND ( 'NONE', #8253, .T. ) ;
#3814 =( BOUNDED_CURVE ( )  B_SPLINE_CURVE ( 2, ( #15292, #7122, #10210, #11897, #16470, #13405, #358, #16565, #2366, #5427, #8727, #16674, #1956, #6810, #2161, #8616, #13295 ),
 .UNSPECIFIED., .F., .F. ) 
 B_SPLINE_CURVE_WITH_KNOTS ( ( 3, 2, 2, 2, 2, 2, 2, 2, 3 ),
 ( 0.6000000000038511194, 0.6125000000038511860, 0.6250000000038511416, 0.6375000000038510972, 0.6500000000038511638, 0.6625000000038511194, 0.6750000000038511860, 0.6875000000038511416, 0.7000000000038510972 ),
 .UNSPECIFIED. ) 
 CURVE ( )  GEOMETRIC_REPRESENTATION_ITEM ( )  RATIONAL_B_SPLINE_CURVE ( ( 0.9999999999940800688, 0.9807852804091503618, 1.000000000000000000, 0.9807852804032304306, 1.000000000000000000, 0.9807852804032304306, 1.000000000000000000, 0.9807852804032304306, 1.000000000000000000, 0.9807852804032304306, 1.000000000000000000, 0.9807852804032304306, 1.000000000000000000, 0.9807852804032304306, 1.000000000000000000, 0.9807852803973104994, 1.000000000005919931 ) ) 
 REPRESENTATION_ITEM ( '' )  );
#3815 = AXIS2_PLACEMENT_3D ( 'NONE', #17913, #305, #7951 ) ;
#3816 = CARTESIAN_POINT ( 'NONE',  ( -2.870125741905209971, 6.929096494179676213, -2.571512499819690767 ) ) ;
#3817 = CARTESIAN_POINT ( 'NONE',  ( 0.000000000000000000, 0.000000000000000000, 0.000000000000000000 ) ) ;
#3818 = DIRECTION ( 'NONE',  ( 0.000000000000000000, 0.000000000000000000, -1.000000000000000000 ) ) ;
#3819 = AXIS2_PLACEMENT_3D ( 'NONE', #582, #18592, #13927 ) ;
#3820 = DIRECTION ( 'NONE',  ( 1.000000000000000000, -0.000000000000000000, -0.000000000000000000 ) ) ;
#3821 = DIRECTION ( 'NONE',  ( -0.000000000000000000, -0.000000000000000000, 1.000000000000000000 ) ) ;
#3822 = CIRCLE ( 'NONE', #10627, 65.24900000006525147 ) ;
#3823 = ORIENTED_EDGE ( 'NONE', *, *, #8501, .F. ) ;
#3824 = CARTESIAN_POINT ( 'NONE',  ( 6.177131623262577698, 10.85999999999999410, 0.000000000000000000 ) ) ;
#3825 = VERTEX_POINT ( 'NONE', #2047 ) ;
#3826 = CARTESIAN_POINT ( 'NONE',  ( 6.888301780572507305, -16.62983158603121936, -5.103862499819686427 ) ) ;
#3827 = CARTESIAN_POINT ( 'NONE',  ( -15.44968093174339963, -14.96845338175447360, 73.80849194119339529 ) ) ;
#3828 = ORIENTED_EDGE ( 'NONE', *, *, #15831, .T. ) ;
#3829 = ADVANCED_FACE ( 'NONE', ( #1746 ), #13188, .T. ) ;
#3830 = CARTESIAN_POINT ( 'NONE',  ( 19.99999999999999645, -64.79224928664389438, 25.14373648582931864 ) ) ;
#3831 = ORIENTED_EDGE ( 'NONE', *, *, #8684, .F. ) ;
#3832 = DIRECTION ( 'NONE',  ( 0.000000000000000000, 0.000000000000000000, 1.000000000000000000 ) ) ;
#3833 = LINE ( 'NONE', #3939, #11727 ) ;
#3834 = EDGE_CURVE ( 'NONE', #20459, #19592, #14902, .T. ) ;
#3835 = VECTOR ( 'NONE', #20140, 1000.000000000000114 ) ;
#3836 = EDGE_LOOP ( 'NONE', ( #8434, #12612, #11629, #11127 ) ) ;
#3837 = AXIS2_PLACEMENT_3D ( 'NONE', #16417, #14627, #8066 ) ;
#3838 = VECTOR ( 'NONE', #6290, 1000.000000000000000 ) ;
#3839 = CARTESIAN_POINT ( 'NONE',  ( 19.99999999999999645, 10.74906464462118372, 71.19310085447972369 ) ) ;
#3840 = CARTESIAN_POINT ( 'NONE',  ( 3.580422610670019878, -18.00000000043040771, -4.809331249819688736 ) ) ;
#3841 = CARTESIAN_POINT ( 'NONE',  ( -4.000000000000000000, 2.309401076758531346, -5.242734410091827613 ) ) ;
#3842 = AXIS2_PLACEMENT_3D ( 'NONE', #1098, #7333, #4370 ) ;
#3843 = CONICAL_SURFACE ( 'NONE', #2846, 2.060000000000000941, 0.9599310885968777018 ) ;
#3844 = DIRECTION ( 'NONE',  ( -1.000000000000000000, -0.000000000000000000, -0.000000000000000000 ) ) ;
#3845 = CARTESIAN_POINT ( 'NONE',  ( -7.902369978624331104, -7.902369976724401113, 10.60198475064743029 ) ) ;
#3846 = ORIENTED_EDGE ( 'NONE', *, *, #18298, .F. ) ;
#3847 = DIRECTION ( 'NONE',  ( 0.000000000000000000, -0.8878852184023794392, 0.4600650377311439887 ) ) ;
#3848 = CYLINDRICAL_SURFACE ( 'NONE', #11531, 11.50000000000000000 ) ;
#3849 = EDGE_LOOP ( 'NONE', ( #17467, #17599, #2886, #15674 ) ) ;
#3850 = VECTOR ( 'NONE', #18373, 1000.000000000000000 ) ;
#3851 = EDGE_CURVE ( 'NONE', #4973, #10522, #11796, .T. ) ;
#3852 = CARTESIAN_POINT ( 'NONE',  ( 0.6949845910673885241, -21.50225451306873836, -70.57937617215435466 ) ) ;
#3853 = ORIENTED_EDGE ( 'NONE', *, *, #1481, .F. ) ;
#3854 = CARTESIAN_POINT ( 'NONE',  ( 10.19618095047497874, -15.25966317163203279, -3.493793749819687378 ) ) ;
#3855 = DIRECTION ( 'NONE',  ( 0.000000000000000000, 0.2697967711570182225, 0.9629172873478010208 ) ) ;
#3856 = LINE ( 'NONE', #15521, #14783 ) ;
#3857 = CIRCLE ( 'NONE', #15722, 65.24900000006523726 ) ;
#3858 = EDGE_LOOP ( 'NONE', ( #15204, #4069, #7384, #9671 ) ) ;
#3859 = CARTESIAN_POINT ( 'NONE',  ( 0.000000000000000000, 0.000000000000000000, 0.000000000000000000 ) ) ;
#3860 = EDGE_LOOP ( 'NONE', ( #4153, #19449 ) ) ;
#3861 = AXIS2_PLACEMENT_3D ( 'NONE', #222, #20895, #12953 ) ;
#3862 = FACE_OUTER_BOUND ( 'NONE', #13317, .T. ) ;
#3863 = VERTEX_POINT ( 'NONE', #11588 ) ;
#3864 = PLANE ( 'NONE',  #1456 ) ;
#3865 = ORIENTED_EDGE ( 'NONE', *, *, #17779, .F. ) ;
#3866 = CARTESIAN_POINT ( 'NONE',  ( 2.339468227445713921, 3.268109542640642573, -5.600000000000002309 ) ) ;
#3867 = EDGE_CURVE ( 'NONE', #5132, #2314, #3722, .T. ) ;
#3868 = DIRECTION ( 'NONE',  ( -1.000000000000000000, 0.000000000000000000, 0.000000000000000000 ) ) ;
#3869 = CARTESIAN_POINT ( 'NONE',  ( -12.54593441764187745, -8.382925368423274293, 10.14419816884154457 ) ) ;
#3870 = ORIENTED_EDGE ( 'NONE', *, *, #6122, .F. ) ;
#3871 = CIRCLE ( 'NONE', #19139, 10.52399999999999558 ) ;
#3872 = DIRECTION ( 'NONE',  ( 0.000000000000000000, 0.000000000000000000, 1.000000000000000000 ) ) ;
#3873 = EDGE_CURVE ( 'NONE', #1539, #8201, #3631, .T. ) ;
#3874 = LINE ( 'NONE', #613, #11834 ) ;
#3875 = CARTESIAN_POINT ( 'NONE',  ( 3.580422614997667896, 17.99999999956958163, 19.34223125018031197 ) ) ;
#3876 = DIRECTION ( 'NONE',  ( 0.5000000000000025535, -0.8660254037844371533, 0.000000000000000000 ) ) ;
#3877 = PRODUCT_DEFINITION_FORMATION_WITH_SPECIFIED_SOURCE ( 'ANY', '', #5599, .NOT_KNOWN. ) ;
#3878 = ORIENTED_EDGE ( 'NONE', *, *, #2731, .F. ) ;
#3879 = DIRECTION ( 'NONE',  ( 0.000000000000000000, 0.9422609221188191775, 0.3348796121709901041 ) ) ;
#3880 = PLANE ( 'NONE',  #9396 ) ;
#3881 = ORIENTED_EDGE ( 'NONE', *, *, #3690, .T. ) ;
#3882 = CARTESIAN_POINT ( 'NONE',  ( -7.500000000000007994, -1.491842754878806687, 11.05666875008779471 ) ) ;
#3883 = EDGE_LOOP ( 'NONE', ( #5778, #20322, #19894, #20334 ) ) ;
#3884 = AXIS2_PLACEMENT_3D ( 'NONE', #2903, #14152, #9682 ) ;
#3885 = CARTESIAN_POINT ( 'NONE',  ( 24.99999999999999645, -39.99999999999999289, -49.89999999999999858 ) ) ;
#3886 = CARTESIAN_POINT ( 'NONE',  ( 12.72792205982779379, -12.72792206288790950, 13.15707500018031162 ) ) ;
#3887 = EDGE_LOOP ( 'NONE', ( #7429, #8836, #13922 ) ) ;
#3888 = ORIENTED_EDGE ( 'NONE', *, *, #6652, .T. ) ;
#3889 = FACE_OUTER_BOUND ( 'NONE', #11532, .T. ) ;
#3890 = EDGE_CURVE ( 'NONE', #3519, #8383, #19747, .T. ) ;
#3891 = EDGE_CURVE ( 'NONE', #12535, #3064, #18640, .T. ) ;
#3892 = DIRECTION ( 'NONE',  ( 0.000000000000000000, 0.9790840876823234673, -0.2034560130526309185 ) ) ;
#3893 = CARTESIAN_POINT ( 'NONE',  ( 0.000000000000000000, 0.000000000000000000, 72.00000000007199219 ) ) ;
#3894 = CARTESIAN_POINT ( 'NONE',  ( 7.500000000000009770, -8.788009009181406898E-15, -12.21129999999768501 ) ) ;
#3895 = UNCERTAINTY_MEASURE_WITH_UNIT (LENGTH_MEASURE( 1.000000000000000082E-05 ), #15899, 'distance_accuracy_value', 'NONE');
#3897 = EDGE_CURVE ( 'NONE', #8714, #17156, #8152, .T. ) ;
#3896 =( LENGTH_UNIT ( ) NAMED_UNIT ( * ) SI_UNIT ( .MILLI., .METRE. ) );
#3898 = CARTESIAN_POINT ( 'NONE',  ( 7.500000000000007994, -9.015933403756345817E-10, -2.786299999819684459 ) ) ;
#3899 = CARTESIAN_POINT ( 'NONE',  ( 6.358192987158596488, -4.248408730893249441, 16.94729375018031448 ) ) ;
#3900 = CIRCLE ( 'NONE', #17469, 205.0000000000000284 ) ;
#3901 = CARTESIAN_POINT ( 'NONE',  ( 6.330490858644138186, 9.474249097082495297, -20.37776600028680818 ) ) ;
#3902 = PRODUCT ( 'BR-546', 'BR-546', '', ( #16504 ) ) ;
#3903 = DIRECTION ( 'NONE',  ( -1.000000000000000000, 0.000000000000000000, 0.000000000000000000 ) ) ;
#3904 = ORIENTED_EDGE ( 'NONE', *, *, #2347, .F. ) ;
#3905 = DIRECTION ( 'NONE',  ( -1.000000000000000000, 0.000000000000000000, -0.000000000000000000 ) ) ;
#3906 = CARTESIAN_POINT ( 'NONE',  ( 16.62983158437509346, -6.888301784570739272, 5.047612500180314044 ) ) ;
#3907 = CYLINDRICAL_SURFACE ( 'NONE', #11657, 72.00000000007199219 ) ;
#3908 = EDGE_CURVE ( 'NONE', #13107, #2970, #10106, .T. ) ;
#3909 = ORIENTED_EDGE ( 'NONE', *, *, #18825, .F. ) ;
#3910 = EDGE_CURVE ( 'NONE', #17156, #8714, #11201, .T. ) ;
#3911 = DIRECTION ( 'NONE',  ( 0.000000000000000000, 0.000000000000000000, 1.000000000000000000 ) ) ;
#3912 = ORIENTED_EDGE ( 'NONE', *, *, #19682, .F. ) ;
#3913 = CYLINDRICAL_SURFACE ( 'NONE', #2759, 27.60000000002759890 ) ;
#3914 = CARTESIAN_POINT ( 'NONE',  ( -44.00000000000000000, -85.00000000000000000, -1.040949779275250179E-14 ) ) ;
#3915 = ORIENTED_EDGE ( 'NONE', *, *, #8388, .F. ) ;
#3916 = ORIENTED_EDGE ( 'NONE', *, *, #3481, .T. ) ;
#3917 = CYLINDRICAL_SURFACE ( 'NONE', #5611, 27.60000000002759890 ) ;
#3918 = AXIS2_PLACEMENT_3D ( 'NONE', #425, #5292, #19912 ) ;
#3919 = ADVANCED_FACE ( 'NONE', ( #17957 ), #3333, .F. ) ;
#3920 =( NAMED_UNIT ( * ) PLANE_ANGLE_UNIT ( ) SI_UNIT ( $, .RADIAN. ) );
#3921 = DIRECTION ( 'NONE',  ( 0.000000000000000000, 0.000000000000000000, 1.000000000000000000 ) ) ;
#3922 = AXIS2_PLACEMENT_3D ( 'NONE', #17466, #5683, #10990 ) ;
#3923 = DIRECTION ( 'NONE',  ( 1.000000000000000000, 0.000000000000000000, 0.000000000000000000 ) ) ;
#3924 = CARTESIAN_POINT ( 'NONE',  ( -2.870125743571140919, -6.929096493489624642, -15.53088749981969308 ) ) ;
#3925 = DIRECTION ( 'NONE',  ( -1.000000000000000000, -0.000000000000000000, -0.000000000000000000 ) ) ;
#3926 = DIRECTION ( 'NONE',  ( -1.000000000000000000, -0.000000000000000000, -0.000000000000000000 ) ) ;
#3927 = CARTESIAN_POINT ( 'NONE',  ( 0.000000000000000000, 0.000000000000000000, 0.000000000000000000 ) ) ;
#3928 = AXIS2_PLACEMENT_3D ( 'NONE', #19077, #4553, #2968 ) ;
#3929 = AXIS2_PLACEMENT_3D ( 'NONE', #19561, #5037, #11500 ) ;
#3930 = ORIENTED_EDGE ( 'NONE', *, *, #18063, .T. ) ;
#3931 = DIRECTION ( 'NONE',  ( 0.000000000000000000, 0.000000000000000000, 1.000000000000000000 ) ) ;
#3932 = ORIENTED_EDGE ( 'NONE', *, *, #2262, .F. ) ;
#3933 = CARTESIAN_POINT ( 'NONE',  ( -6.888301784570738384, -16.62983158437509346, 5.499262500180314817 ) ) ;
#3934 = CARTESIAN_POINT ( 'NONE',  ( -65.00002539999999840, 0.000000000000000000, 0.000000000000000000 ) ) ;
#3935 = ORIENTED_EDGE ( 'NONE', *, *, #17793, .T. ) ;
#3936 = CARTESIAN_POINT ( 'NONE',  ( 19.99999999999999645, -54.08351995568730786, 35.76369202524482915 ) ) ;
#3937 = EDGE_LOOP ( 'NONE', ( #5520, #480, #4060, #3025 ) ) ;
#3938 = CARTESIAN_POINT ( 'NONE',  ( 41.22647390543421864, -123.0286131151452196, 80.84140696824476890 ) ) ;
#3939 = CARTESIAN_POINT ( 'NONE',  ( 50.00000000000000000, -105.0000000000000426, 77.45966692414833688 ) ) ;
#3940 = AXIS2_PLACEMENT_3D ( 'NONE', #15189, #10205, #12117 ) ;
#3941 = ORIENTED_EDGE ( 'NONE', *, *, #6424, .F. ) ;
#3942 = LINE ( 'NONE', #10430, #19155 ) ;
#3943 = AXIS2_PLACEMENT_3D ( 'NONE', #3662, #5256, #1981 ) ;
#3944 =( BOUNDED_CURVE ( )  B_SPLINE_CURVE ( 2, ( #4637, #777, #19661, #13824, #13210, #10031, #2687, #998, #5141, #1977, #2583, #7442, #17212, #16496, #9148, #5530, #20372 ),
 .UNSPECIFIED., .F., .T. ) 
 B_SPLINE_CURVE_WITH_KNOTS ( ( 3, 2, 2, 2, 2, 2, 2, 2, 3 ),
 ( 0.9000000000038511638, 0.9125000000033697267, 0.9250000000028884006, 0.9375000000024069635, 0.9500000000019255264, 0.9625000000014442003, 0.9750000000009627632, 0.9875000000004814371, 1.000000000000000000 ),
 .UNSPECIFIED. ) 
 CURVE ( )  GEOMETRIC_REPRESENTATION_ITEM ( )  RATIONAL_B_SPLINE_CURVE ( ( 0.9999999999940800688, 0.9807852804091503618, 1.000000000000000000, 0.9807852804032304306, 1.000000000000000000, 0.9807852804032304306, 1.000000000000000000, 0.9807852804032304306, 1.000000000000000000, 0.9807852804032304306, 1.000000000000000000, 0.9807852804032304306, 1.000000000000000000, 0.9807852804032304306, 1.000000000000000000, 0.9807852804032304306, 1.000000000000000000 ) ) 
 REPRESENTATION_ITEM ( '' )  );
#3945 = CARTESIAN_POINT ( 'NONE',  ( 19.99999999999999645, 0.000000000000000000, 0.000000000000000000 ) ) ;
#3946 = CARTESIAN_POINT ( 'NONE',  ( -2.163827323447877821E-09, -17.99999999999999645, -4.514799999819691934 ) ) ;
#3947 = DIRECTION ( 'NONE',  ( -1.000000000000000000, 0.000000000000000000, 0.000000000000000000 ) ) ;
#3948 = VECTOR ( 'NONE', #2830, 1000.000000000000000 ) ;
#3949 = CIRCLE ( 'NONE', #7006, 5.000000000000004441 ) ;
#3950 = FACE_OUTER_BOUND ( 'NONE', #17672, .T. ) ;
#3951 = CARTESIAN_POINT ( 'NONE',  ( 4.276731815070943910, 10.32494394706616703, 5.300422250647430111 ) ) ;
#3952 = ORIENTED_EDGE ( 'NONE', *, *, #3142, .F. ) ;
#3953 = DIRECTION ( 'NONE',  ( 1.000000000000000000, -0.000000000000000000, -0.000000000000000000 ) ) ;
#3954 = EDGE_CURVE ( 'NONE', #10395, #6717, #6916, .T. ) ;
#3955 = PLANE ( 'NONE',  #15253 ) ;
#3956 = ORIENTED_EDGE ( 'NONE', *, *, #10477, .T. ) ;
#3957 = AXIS2_PLACEMENT_3D ( 'NONE', #5817, #18649, #2969 ) ;
#3958 = CARTESIAN_POINT ( 'NONE',  ( 14.87228507261737853, -15.53036221685706408, -73.48983352790762069 ) ) ;
#3959 = ORIENTED_EDGE ( 'NONE', *, *, #13412, .F. ) ;
#3960 = AXIS2_PLACEMENT_3D ( 'NONE', #13193, #19641, #48 ) ;
#3961 = CARTESIAN_POINT ( 'NONE',  ( 18.00000000000000000, -2.163824016901520184E-09, 13.88355000018031404 ) ) ;
#3962 = DIRECTION ( 'NONE',  ( -1.000000000000000000, -0.000000000000000000, -0.000000000000000000 ) ) ;
#3963 = CARTESIAN_POINT ( 'NONE',  ( 24.99999999999999645, -122.0000000000000000, 2.099999999999991207 ) ) ;
#3964 = VERTEX_POINT ( 'NONE', #16165 ) ;
#3965 = AXIS2_PLACEMENT_3D ( 'NONE', #7865, #12763, #2890 ) ;
#3966 = CARTESIAN_POINT ( 'NONE',  ( 0.000000000000000000, 71.76067541710851572, 5.865617076724869428 ) ) ;
#3967 = ORIENTED_EDGE ( 'NONE', *, *, #13897, .F. ) ;
#3968 = CARTESIAN_POINT ( 'NONE',  ( 0.000000000000000000, 0.000000000000000000, 0.000000000000000000 ) ) ;
#3969 = AXIS2_PLACEMENT_3D ( 'NONE', #18081, #19560, #10125 ) ;
#3970 = VERTEX_POINT ( 'NONE', #19637 ) ;
#3971 = DIRECTION ( 'NONE',  ( 0.000000000000000000, 0.9422609221188213979, -0.3348796121709836648 ) ) ;
#3972 = VECTOR ( 'NONE', #20531, 1000.000000000000000 ) ;
#3973 = ORIENTED_EDGE ( 'NONE', *, *, #18256, .F. ) ;
#3974 = CARTESIAN_POINT ( 'NONE',  ( 30.00000000000000000, -40.41646384503850697, -66.42520834682599684 ) ) ;
#3975 = FACE_OUTER_BOUND ( 'NONE', #14612, .T. ) ;
#3976 = ITEM_DEFINED_TRANSFORMATION ( 'NONE', 'NONE', #18481,  #12461 ) ;
#3977 = CARTESIAN_POINT ( 'NONE',  ( 18.00000000000000355, -2.163824016901520597E-09, -23.81644999981969590 ) ) ;
#3978 = ORIENTED_EDGE ( 'NONE', *, *, #1009, .F. ) ;
#3979 = EDGE_CURVE ( 'NONE', #9694, #4085, #257, .T. ) ;
#3980 = DIRECTION ( 'NONE',  ( -0.000000000000000000, -0.000000000000000000, 1.000000000000000000 ) ) ;
#3981 = ORIENTED_EDGE ( 'NONE', *, *, #3851, .T. ) ;
#3982 = DIRECTION ( 'NONE',  ( 0.000000000000000000, -0.9976687691905385957, -0.06824241336468162000 ) ) ;
#3983 = CARTESIAN_POINT ( 'NONE',  ( -13.67243654778935102, -5.663308646854334327, -23.45435441848093561 ) ) ;
#3984 = DIRECTION ( 'NONE',  ( -1.000000000000000000, 0.000000000000000000, 0.000000000000000000 ) ) ;
#3985 = EDGE_CURVE ( 'NONE', #7047, #4150, #1949, .T. ) ;
#3986 = ORIENTED_EDGE ( 'NONE', *, *, #14658, .T. ) ;
#3987 = CARTESIAN_POINT ( 'NONE',  ( 30.32166929073842709, -108.6878471672527269, 78.46984228986231358 ) ) ;
#3988 = CARTESIAN_POINT ( 'NONE',  ( -0.3263565795980851170, 4.430380094434251959, -5.351519936624993257 ) ) ;
#3989 = ORIENTED_EDGE ( 'NONE', *, *, #17647, .F. ) ;
#3990 = CARTESIAN_POINT ( 'NONE',  ( -6.043644376632333781, -22.24467714164983079, -75.70091669079042163 ) ) ;
#3991 = VERTEX_POINT ( 'NONE', #13086 ) ;
#3992 = LINE ( 'NONE', #15233, #8841 ) ;
#3993 = CARTESIAN_POINT ( 'NONE',  ( 16.62983158603121936, 6.888301780572501976, 11.38988750018031126 ) ) ;
#3994 = EDGE_LOOP ( 'NONE', ( #9300, #8665, #12301, #14059 ) ) ;
#3995 = EDGE_LOOP ( 'NONE', ( #19762, #3330, #9556, #15232 ) ) ;
#3996 = DIRECTION ( 'NONE',  ( 0.000000000000000000, -9.714451465470119729E-15, -1.000000000000000000 ) ) ;
#3997 = DIRECTION ( 'NONE',  ( -1.000000000000000000, 0.000000000000000000, -0.000000000000000000 ) ) ;
#3998 = CARTESIAN_POINT ( 'NONE',  ( 150.0000507999999968, 5.400000000000000355, -1.000000000000000000 ) ) ;
#3999 = CARTESIAN_POINT ( 'NONE',  ( 6.358192988180019434, 4.248408729364581582, -13.09489374981968801 ) ) ;
#4000 = SURFACE_STYLE_USAGE ( .BOTH. , #8460 ) ;
#4001 = CARTESIAN_POINT ( 'NONE',  ( 6.358192987158595599, -4.248408730893249441, -1.902706249819686279 ) ) ;
#4002 = DIRECTION ( 'NONE',  ( 1.000000000000000000, 0.000000000000000000, 0.000000000000000000 ) ) ;
#4003 = CARTESIAN_POINT ( 'NONE',  ( -11.17563879758427525, -2.222972768810838051, -14.48714100028680463 ) ) ;
#4004 = DIRECTION ( 'NONE',  ( -1.000000000000000000, 0.000000000000000000, 0.000000000000000000 ) ) ;
#4005 = EDGE_CURVE ( 'NONE', #5332, #19322, #8478, .T. ) ;
#4006 = EDGE_CURVE ( 'NONE', #231, #6577, #16940, .T. ) ;
#4007 = ORIENTED_EDGE ( 'NONE', *, *, #6895, .F. ) ;
#4008 = CARTESIAN_POINT ( 'NONE',  ( -6.359999999999997655, 4.663913298532544267E-15, 0.000000000000000000 ) ) ;
#4009 = EDGE_CURVE ( 'NONE', #17803, #15688, #12905, .T. ) ;
#4010 = CARTESIAN_POINT ( 'NONE',  ( -10.19618095047498052, 15.25966317163203101, -8.206293749819685956 ) ) ;
#4011 = CARTESIAN_POINT ( 'NONE',  ( -10.00000000000000000, 0.000000000000000000, 0.000000000000000000 ) ) ;
#4012 = ORIENTED_EDGE ( 'NONE', *, *, #14999, .F. ) ;
#4013 = DIRECTION ( 'NONE',  ( 1.000000000000000000, 0.000000000000000000, 0.000000000000000000 ) ) ;
#4014 = VERTEX_POINT ( 'NONE', #16776 ) ;
#4015 = CARTESIAN_POINT ( 'NONE',  ( -24.99999999999999289, -1.326995226329896749, 84.99999999999998579 ) ) ;
#4017 = EDGE_CURVE ( 'NONE', #20752, #13475, #15503, .T. ) ;
#4016 = FACE_BOUND ( 'NONE', #2402, .T. ) ;
#4018 = VERTEX_POINT ( 'NONE', #5639 ) ;
#4019 = EDGE_CURVE ( 'NONE', #7176, #5705, #17962, .T. ) ;
#4020 = EDGE_LOOP ( 'NONE', ( #17875, #1699, #5148, #10890, #3930, #12692 ) ) ;
#4021 = DIRECTION ( 'NONE',  ( -1.000000000000000000, 0.000000000000000000, -0.000000000000000000 ) ) ;
#4022 = VECTOR ( 'NONE', #16126, 1000.000000000000000 ) ;
#4023 = PRODUCT_DEFINITION ( 'UNKNOWN', '', #3550, #5590 ) ;
#4024 =( LENGTH_UNIT ( ) NAMED_UNIT ( * ) SI_UNIT ( .MILLI., .METRE. ) );
#4025 = CARTESIAN_POINT ( 'NONE',  ( 10.00000000000000178, -164.9999999999999716, -70.00000000000000000 ) ) ;
#4026 = DIRECTION ( 'NONE',  ( -0.000000000000000000, -0.000000000000000000, 1.000000000000000000 ) ) ;
#4027 = EDGE_CURVE ( 'NONE', #10832, #7909, #15086, .T. ) ;
#4028 = CARTESIAN_POINT ( 'NONE',  ( -4.248408730893245000, -6.358192987158590270, -5.811356249819689346 ) ) ;
#4029 = CARTESIAN_POINT ( 'NONE',  ( 19.99999999999999645, -19.38316218894255627, 61.87375713200982119 ) ) ;
#4030 = DIRECTION ( 'NONE',  ( 1.000000000000000000, 0.000000000000000000, 0.000000000000000000 ) ) ;
#4031 = CARTESIAN_POINT ( 'NONE',  ( 0.000000000000000000, -1.178949249685218303, -2.041999999999998039 ) ) ;
#4032 = CARTESIAN_POINT ( 'NONE',  ( 50.00000000000000000, 230.0000000000000000, 0.000000000000000000 ) ) ;
#4033 = EDGE_CURVE ( 'NONE', #5350, #1631, #944, .T. ) ;
#4034 = CIRCLE ( 'NONE', #13874, 2.649999999999993694 ) ;
#4035 = EDGE_LOOP ( 'NONE', ( #4943, #19374, #15478 ) ) ;
#4036 = DIRECTION ( 'NONE',  ( 0.000000000000000000, -0.4999999999999993339, 0.8660254037844390407 ) ) ;
#4037 = ADVANCED_FACE ( 'NONE', ( #8928 ), #15283, .T. ) ;
#4038 = ORIENTED_EDGE ( 'NONE', *, *, #1490, .T. ) ;
#4039 = CARTESIAN_POINT ( 'NONE',  ( -16.62983158603122291, -6.888301780572501087, -2.747612499819685805 ) ) ;
#4040 = CARTESIAN_POINT ( 'NONE',  ( 5.982253535725046589, -20.70709046307244350, 70.91533586927069166 ) ) ;
#4041 = VERTEX_POINT ( 'NONE', #4155 ) ;
#4042 = CARTESIAN_POINT ( 'NONE',  ( 30.00000000000000000, -30.00000000000000711, 58.09475019311124555 ) ) ;
#4043 = ORIENTED_EDGE ( 'NONE', *, *, #8330, .F. ) ;
#4044 = EDGE_CURVE ( 'NONE', #10942, #3107, #12216, .T. ) ;
#4045 = CARTESIAN_POINT ( 'NONE',  ( 0.000000000000000000, 0.000000000000000000, 0.000000000000000000 ) ) ;
#4046 = FACE_OUTER_BOUND ( 'NONE', #5304, .T. ) ;
#4047 = ORIENTED_EDGE ( 'NONE', *, *, #14962, .F. ) ;
#4048 = DIRECTION ( 'NONE',  ( -1.000000000000000000, -0.000000000000000000, -0.000000000000000000 ) ) ;
#4049 = DIRECTION ( 'NONE',  ( -1.000000000000000000, 0.000000000000000000, -0.000000000000000000 ) ) ;
#4050 = CARTESIAN_POINT ( 'NONE',  ( -6.888301784570736608, -16.62983158437509346, -3.925737499819691223 ) ) ;
#4051 = CYLINDRICAL_SURFACE ( 'NONE', #16717, 14.49999999999999822 ) ;
#4052 = CARTESIAN_POINT ( 'NONE',  ( 2.500000000000000000, -1.178949249685214307, 2.042000000000001592 ) ) ;
#4053 = CARTESIAN_POINT ( 'NONE',  ( -1.343452921478824119E-09, -11.17563879731705789, -18.85114024935257149 ) ) ;
#4054 = ORIENTED_EDGE ( 'NONE', *, *, #2200, .T. ) ;
#4055 = ADVANCED_FACE ( 'NONE', ( #5526 ), #10638, .T. ) ;
#4056 = FACE_OUTER_BOUND ( 'NONE', #17062, .T. ) ;
#4057 = AXIS2_PLACEMENT_3D ( 'NONE', #16449, #1936, #8393 ) ;
#4058 = EDGE_LOOP ( 'NONE', ( #8111, #19918 ) ) ;
#4059 = DIRECTION ( 'NONE',  ( 0.000000000000000000, 0.000000000000000000, -1.000000000000000000 ) ) ;
#4060 = ORIENTED_EDGE ( 'NONE', *, *, #1446, .T. ) ;
#4061 = CARTESIAN_POINT ( 'NONE',  ( -18.00000000000000000, 2.163826221265758884E-09, -0.2539499998196886876 ) ) ;
#4062 = DIRECTION ( 'NONE',  ( -1.000000000000000000, 0.000000000000000000, -0.000000000000000000 ) ) ;
#4063 = CARTESIAN_POINT ( 'NONE',  ( 50.00000000000000000, -1.326995226329893862, 84.99999999999998579 ) ) ;
#4064 = EDGE_LOOP ( 'NONE', ( #13615, #9861, #16001, #19899 ) ) ;
#4065 = DIRECTION ( 'NONE',  ( 0.000000000000000000, 0.1361666490962400722, 0.9906859460363316439 ) ) ;
#4066 = EDGE_LOOP ( 'NONE', ( #15507, #11578, #6536, #20580 ) ) ;
#4067 = CARTESIAN_POINT ( 'NONE',  ( -7.500000000000007994, 1.491842755816070287, 11.64573125008779186 ) ) ;
#4068 = AXIS2_PLACEMENT_3D ( 'NONE', #18351, #11993, #5102 ) ;
#4069 = ORIENTED_EDGE ( 'NONE', *, *, #12570, .T. ) ;
#4070 = DIRECTION ( 'NONE',  ( 0.000000000000000000, 0.000000000000000000, 1.000000000000000000 ) ) ;
#4071 = ADVANCED_FACE ( 'NONE', ( #773 ), #7223, .F. ) ;
#4072 = AXIS2_PLACEMENT_3D ( 'NONE', #17732, #8083, #3398 ) ;
#4073 = DIRECTION ( 'NONE',  ( 1.000000000000000000, -0.000000000000000000, -0.000000000000000000 ) ) ;
#4074 = PRODUCT_DEFINITION_SHAPE ( 'NONE', 'NONE',  #20958 ) ;
#4075 = CYLINDRICAL_SURFACE ( 'NONE', #14992, 5.000000000000004441 ) ;
#4076 = CONTEXT_DEPENDENT_SHAPE_REPRESENTATION ( #9140, #12215 ) ;
#4077 = CARTESIAN_POINT ( 'NONE',  ( -13.67243654642775574, 5.663308650141533285, 2.191854418841544749 ) ) ;
#4078 = ORIENTED_EDGE ( 'NONE', *, *, #19175, .T. ) ;
#4079 = CARTESIAN_POINT ( 'NONE',  ( 24.74873734152916072, 24.74873734152916072, -130.0000000000000000 ) ) ;
#4080 = ORIENTED_EDGE ( 'NONE', *, *, #10392, .F. ) ;
#4081 = CARTESIAN_POINT ( 'NONE',  ( -21.18805271706017379, -3.649167310370820871, 90.00000000000000000 ) ) ;
#4082 = CARTESIAN_POINT ( 'NONE',  ( 15.25966317163202568, 10.19618095047498230, 20.52035625018031340 ) ) ;
#4083 = LINE ( 'NONE', #7161, #2116 ) ;
#4084 = CIRCLE ( 'NONE', #12565, 11.49999999999999467 ) ;
#4085 = VERTEX_POINT ( 'NONE', #18364 ) ;
#4086 = DIRECTION ( 'NONE',  ( -1.000000000000000000, -0.000000000000000000, -0.000000000000000000 ) ) ;
#4087 = CARTESIAN_POINT ( 'NONE',  ( 0.000000000000000000, 19.38316218894212639, 61.87375713200996330 ) ) ;
#4088 = EDGE_LOOP ( 'NONE', ( #12384, #14226, #7359, #16071 ) ) ;
#4089 = CARTESIAN_POINT ( 'NONE',  ( 16.72766586881387951, -15.78946417207352226, -79.16083386016902068 ) ) ;
#4090 = ORIENTED_EDGE ( 'NONE', *, *, #4414, .T. ) ;
#4091 = CARTESIAN_POINT ( 'NONE',  ( -2.870125743571141808, -6.929096493489625530, 3.319112500180309233 ) ) ;
#4092 = CARTESIAN_POINT ( 'NONE',  ( 16.62983158437509346, -6.888301784570737496, -15.70698749981969122 ) ) ;
#4093 = EDGE_CURVE ( 'NONE', #14747, #10832, #17096, .T. ) ;
#4094 = ORIENTED_EDGE ( 'NONE', *, *, #16869, .T. ) ;
#4095 = ORIENTED_EDGE ( 'NONE', *, *, #15439, .T. ) ;
#4096 = DIRECTION ( 'NONE',  ( -0.000000000000000000, -1.000000000000000000, -0.000000000000000000 ) ) ;
#4097 = AXIS2_PLACEMENT_3D ( 'NONE', #13900, #19096, #20573 ) ;
#4098 = AXIS2_PLACEMENT_3D ( 'NONE', #7377, #822, #18620 ) ;
#4099 = FACE_BOUND ( 'NONE', #8086, .T. ) ;
#4100 = DIRECTION ( 'NONE',  ( 0.000000000000000000, 0.000000000000000000, -1.000000000000000000 ) ) ;
#4101 = DIRECTION ( 'NONE',  ( 0.000000000000000000, 0.000000000000000000, 1.000000000000000000 ) ) ;
#4102 = AXIS2_PLACEMENT_3D ( 'NONE', #14527, #4870, #16409 ) ;
#4103 = FILL_AREA_STYLE ('',( #15241 ) ) ;
#4104 = DIRECTION ( 'NONE',  ( -1.000000000000000000, -0.000000000000000000, -0.000000000000000000 ) ) ;
#4105 = UNCERTAINTY_MEASURE_WITH_UNIT (LENGTH_MEASURE( 1.000000000000000082E-05 ), #6532, 'distance_accuracy_value', 'NONE');
#4106 = PLANE ( 'NONE',  #8282 ) ;
#4107 = CARTESIAN_POINT ( 'NONE',  ( -6.929096493489632635, 2.870125743571140919, -6.909737499819684992 ) ) ;
#4108 =( REPRESENTATION_RELATIONSHIP ('NONE','NONE', #13739, #12383 ) REPRESENTATION_RELATIONSHIP_WITH_TRANSFORMATION ( #4510 )SHAPE_REPRESENTATION_RELATIONSHIP( ) );
#4109 = AXIS2_PLACEMENT_3D ( 'NONE', #9131, #15270, #15384 ) ;
#4110 = CYLINDRICAL_SURFACE ( 'NONE', #18878, 2.649999999999999467 ) ;
#4111 = CARTESIAN_POINT ( 'NONE',  ( -6.330490858644137298, -9.474249097082495297, -25.09026600028681031 ) ) ;
#4112 = FACE_BOUND ( 'NONE', #15261, .T. ) ;
#4113 = VECTOR ( 'NONE', #2918, 1000.000000000000000 ) ;
#4114 = AXIS2_PLACEMENT_3D ( 'NONE', #1940, #8803, #5220 ) ;
#4115 = ORIENTED_EDGE ( 'NONE', *, *, #17918, .F. ) ;
#4116 = CARTESIAN_POINT ( 'NONE',  ( 0.000000000000000000, 0.000000000000000000, 40.00000000000000000 ) ) ;
#4117 = CARTESIAN_POINT ( 'NONE',  ( 6.888301780572507305, -16.62983158603121936, -12.62426249981968596 ) ) ;
#4118 = CARTESIAN_POINT ( 'NONE',  ( 6.250000000000054179, 10.82531754730546147, 46.00000000000000711 ) ) ;
#4119 = AXIS2_PLACEMENT_3D ( 'NONE', #4445, #10913, #20560 ) ;
#4120 = VERTEX_POINT ( 'NONE', #10204 ) ;
#4121 = DIRECTION ( 'NONE',  ( -1.000000000000000000, 8.881784197001252323E-16, 0.000000000000000000 ) ) ;
#4122 = ORIENTED_EDGE ( 'NONE', *, *, #15323, .F. ) ;
#4123 = CARTESIAN_POINT ( 'NONE',  ( 30.00000000000000000, -39.99999999999999289, 52.00000000000000000 ) ) ;
#4124 = DIRECTION ( 'NONE',  ( 0.000000000000000000, 0.8169698930104393186, 0.5766803221148710801 ) ) ;
#4125 = EDGE_LOOP ( 'NONE', ( #9380, #6892, #547, #14561 ) ) ;
#4126 = VERTEX_POINT ( 'NONE', #16667 ) ;
#4127 = DIRECTION ( 'NONE',  ( -1.000000000000000000, 0.000000000000000000, 0.000000000000000000 ) ) ;
#4128 = FACE_OUTER_BOUND ( 'NONE', #4604, .T. ) ;
#4129 = AXIS2_PLACEMENT_3D ( 'NONE', #15461, #15554, #1050 ) ;
#4130 = EDGE_CURVE ( 'NONE', #18621, #11808, #20663, .T. ) ;
#4131 = CIRCLE ( 'NONE', #10575, 27.60000000002760245 ) ;
#4132 = ADVANCED_FACE ( 'NONE', ( #882 ), #7022, .F. ) ;
#4133 = CARTESIAN_POINT ( 'NONE',  ( -25.00000000000000000, -30.00000000000000711, 58.09475019311124555 ) ) ;
#4134 = AXIS2_PLACEMENT_3D ( 'NONE', #4944, #4529, #3351 ) ;
#4135 = CARTESIAN_POINT ( 'NONE',  ( -1.491842754445841246, 7.500000000179339210, -2.276981249819689967 ) ) ;
#4136 = B_SPLINE_CURVE_WITH_KNOTS ( 'NONE', 3,
 ( #8171, #19611, #7975, #12955 ),
 .UNSPECIFIED., .F., .F.,
 ( 4, 4 ),
 ( 2.380737581620991176E-07, 0.002336974151641539946 ),
 .UNSPECIFIED. ) ;
#4137 = CARTESIAN_POINT ( 'NONE',  ( -24.99999999999999289, 230.0000000000000000, -85.00000000000000000 ) ) ;
#4138 = EDGE_CURVE ( 'NONE', #17904, #1745, #14593, .T. ) ;
#4139 = CARTESIAN_POINT ( 'NONE',  ( -21.50000000000000000, 2.632990618166809235E-15, 68.00000000000000000 ) ) ;
#4140 = CIRCLE ( 'NONE', #14986, 27.60000000002760245 ) ;
#4141 = FACE_OUTER_BOUND ( 'NONE', #16696, .T. ) ;
#4142 = CARTESIAN_POINT ( 'NONE',  ( -7.500000000000000000, 0.000000000000000000, 166.0000000000000000 ) ) ;
#4143 = EDGE_CURVE ( 'NONE', #6043, #11637, #20263, .T. ) ;
#4144 = VERTEX_POINT ( 'NONE', #20044 ) ;
#4145 = DIRECTION ( 'NONE',  ( 0.000000000000000000, -1.224646799147353454E-16, 1.000000000000000000 ) ) ;
#4146 = EDGE_LOOP ( 'NONE', ( #19786, #5788, #5231 ) ) ;
#4147 = CARTESIAN_POINT ( 'NONE',  ( 12.72792206288790950, 12.72792205982780089, 1.375825000180314728 ) ) ;
#4148 = CARTESIAN_POINT ( 'NONE',  ( -19.93133741578929730, -8.067442883292187616, 78.55234307929261206 ) ) ;
#4149 = CIRCLE ( 'NONE', #8544, 2.649999999999999467 ) ;
#4150 = VERTEX_POINT ( 'NONE', #12006 ) ;
#4151 = VECTOR ( 'NONE', #19677, 1000.000000000000000 ) ;
#4152 = CYLINDRICAL_SURFACE ( 'NONE', #17397, 72.00000000007199219 ) ;
#4153 = ORIENTED_EDGE ( 'NONE', *, *, #11160, .F. ) ;
#4154 = TOROIDAL_SURFACE ( 'NONE', #444, 4.000000000000000000, 0.2500000000000000000 ) ;
#4155 = CARTESIAN_POINT ( 'NONE',  ( 30.00000000000000000, -148.4917293642369884, -48.67032260359990659 ) ) ;
#4156 = CARTESIAN_POINT ( 'NONE',  ( 19.99999999999999645, 0.000000000000000000, 0.000000000000000000 ) ) ;
#4157 = CARTESIAN_POINT ( 'NONE',  ( -8.999999999999987566, -85.00000000000000000, 5.000000000000000000 ) ) ;
#4158 = VERTEX_POINT ( 'NONE', #18474 ) ;
#4159 = CARTESIAN_POINT ( 'NONE',  ( -26.35784117651625280, 26.35784117651607872, -120.0000000000000142 ) ) ;
#4160 = EDGE_CURVE ( 'NONE', #19413, #13015, #10425, .T. ) ;
#4161 = VECTOR ( 'NONE', #15732, 1000.000000000000000 ) ;
#4162 = DIRECTION ( 'NONE',  ( 1.000000000000000000, 0.000000000000000000, 0.000000000000000000 ) ) ;
#4163 = CARTESIAN_POINT ( 'NONE',  ( 17.99999999956957808, -3.580422614997675446, -6.576518749819691756 ) ) ;
#4164 = LINE ( 'NONE', #671, #6564 ) ;
#4165 = VECTOR ( 'NONE', #2764, 1000.000000000000114 ) ;
#4166 = ADVANCED_FACE ( 'NONE', ( #9144 ), #16601, .F. ) ;
#4167 = EDGE_CURVE ( 'NONE', #9436, #10849, #999, .T. ) ;
#4168 = CARTESIAN_POINT ( 'NONE',  ( 25.00000000000000000, -30.00000000000000711, -50.99019513592786268 ) ) ;
#4169 = CARTESIAN_POINT ( 'NONE',  ( 7.902369978624329327, 7.902369976724401113, -3.535515249352572997 ) ) ;
#4171 = ORIENTED_EDGE ( 'NONE', *, *, #20774, .T. ) ;
#4170 = AXIS2_PLACEMENT_3D ( 'NONE', #5327, #18362, #16977 ) ;
#4172 = CARTESIAN_POINT ( 'NONE',  ( 0.000000000000000000, 0.000000000000000000, 0.000000000000000000 ) ) ;
#4173 = ADVANCED_FACE ( 'NONE', ( #1100 ), #9827, .T. ) ;
#4174 = CARTESIAN_POINT ( 'NONE',  ( 0.000000000000000000, 0.000000000000000000, 126.0000000000000000 ) ) ;
#4175 = VERTEX_POINT ( 'NONE', #20587 ) ;
#4176 = CARTESIAN_POINT ( 'NONE',  ( 11.44271251907791687, -18.21718295280815880, -72.06823551977505815 ) ) ;
#4177 = EDGE_LOOP ( 'NONE', ( #10550, #12157 ) ) ;
#4178 = CARTESIAN_POINT ( 'NONE',  ( -6.888301780572501976, 16.62983158603122291, -17.33676249981968809 ) ) ;
#4179 = CYLINDRICAL_SURFACE ( 'NONE', #16838, 10.00000000000000178 ) ;
#4180 = DIRECTION ( 'NONE',  ( 0.000000000000000000, 0.000000000000000000, 1.000000000000000000 ) ) ;
#4181 = CIRCLE ( 'NONE', #8931, 5.000000000000004441 ) ;
#4182 = ORIENTED_EDGE ( 'NONE', *, *, #1730, .T. ) ;
#4183 = AXIS2_PLACEMENT_3D ( 'NONE', #6641, #16394, #11623 ) ;
#4184 = VECTOR ( 'NONE', #17323, 1000.000000000000000 ) ;
#4185 = LINE ( 'NONE', #5885, #12633 ) ;
#4186 = VERTEX_POINT ( 'NONE', #14135 ) ;
#4187 = CYLINDRICAL_SURFACE ( 'NONE', #3774, 11.50000000000000000 ) ;
#4188 = EDGE_CURVE ( 'NONE', #4388, #19414, #11152, .T. ) ;
#4189 = ORIENTED_EDGE ( 'NONE', *, *, #8496, .F. ) ;
#4190 = VECTOR ( 'NONE', #3319, 1000.000000000000000 ) ;
#4191 = AXIS2_PLACEMENT_3D ( 'NONE', #1821, #11464, #3201 ) ;
#4192 = EDGE_CURVE ( 'NONE', #17681, #141, #12762, .T. ) ;
#4193 = CARTESIAN_POINT ( 'NONE',  ( 0.000000000000000000, 28.84646472442454979, 58.52617768068444093 ) ) ;
#4194 = EDGE_CURVE ( 'NONE', #3467, #17864, #1526, .T. ) ;
#4195 = CYLINDRICAL_SURFACE ( 'NONE', #4491, 7.500000000000000000 ) ;
#4196 = CIRCLE ( 'NONE', #1175, 4.250000000000000000 ) ;
#4197 = CARTESIAN_POINT ( 'NONE',  ( 10.46442989454075700, 10.46442989202484419, -4.287833081158456849 ) ) ;
#4198 = AXIS2_PLACEMENT_3D ( 'NONE', #15124, #3980, #3761 ) ;
#4199 = ORIENTED_EDGE ( 'NONE', *, *, #6272, .T. ) ;
#4200 = CARTESIAN_POINT ( 'NONE',  ( 19.99999999999999645, -10.74906464462069167, -71.19310085447979475 ) ) ;
#4201 = ORIENTED_EDGE ( 'NONE', *, *, #16066, .F. ) ;
#4202 = LINE ( 'NONE', #13851, #13194 ) ;
#4203 = CARTESIAN_POINT ( 'NONE',  ( 12.72792205982779379, -12.72792206288790950, 3.732075000180308688 ) ) ;
#4204 = CIRCLE ( 'NONE', #3194, 27.60000000002759890 ) ;
#4205 = FACE_OUTER_BOUND ( 'NONE', #18159, .T. ) ;
#4206 = CARTESIAN_POINT ( 'NONE',  ( 1.321505333908969293, -3.855830693249186147, -5.565789719053443996 ) ) ;
#4207 = ORIENTED_EDGE ( 'NONE', *, *, #15117, .F. ) ;
#4208 = DIRECTION ( 'NONE',  ( -0.000000000000000000, 0.000000000000000000, 1.000000000000000000 ) ) ;
#4209 = DIRECTION ( 'NONE',  ( 1.000000000000000000, 0.000000000000000000, -0.000000000000000000 ) ) ;
#4210 = VECTOR ( 'NONE', #11263, 1000.000000000000000 ) ;
#4211 = ORIENTED_EDGE ( 'NONE', *, *, #16340, .F. ) ;
#4212 = CARTESIAN_POINT ( 'NONE',  ( 22.55358526068749114, -4.614239574836358493, -88.80301248374354373 ) ) ;
#4213 = ORIENTED_EDGE ( 'NONE', *, *, #13328, .F. ) ;
#4214 = DIRECTION ( 'NONE',  ( 0.000000000000000000, 1.000000000000000000, 0.000000000000000000 ) ) ;
#4215 = CARTESIAN_POINT ( 'NONE',  ( -17.99999999956958163, 3.580422614997673669, -20.71401874981969371 ) ) ;
#4216 = ORIENTED_EDGE ( 'NONE', *, *, #7272, .F. ) ;
#4217 = VERTEX_POINT ( 'NONE', #9557 ) ;
#4218 = CARTESIAN_POINT ( 'NONE',  ( -44.00000000000000000, -85.00000000000000000, -1.040949779275250179E-14 ) ) ;
#4219 = VECTOR ( 'NONE', #16881, 1000.000000000000000 ) ;
#4220 = CARTESIAN_POINT ( 'NONE',  ( 9.999999999999998224, 64.36139404985965484, 32.27399814043898374 ) ) ;
#4221 = CYLINDRICAL_SURFACE ( 'NONE', #12418, 65.24900000006525147 ) ;
#4222 = DIRECTION ( 'NONE',  ( 0.000000000000000000, 0.000000000000000000, 1.000000000000000000 ) ) ;
#4223 = PRESENTATION_STYLE_ASSIGNMENT (( #7073 ) ) ;
#4224 = CARTESIAN_POINT ( 'NONE',  ( 3.580422614997669228, 17.99999999956958874, 2.396831250180309070 ) ) ;
#4225 = CARTESIAN_POINT ( 'NONE',  ( 6.358192987158595599, -4.248408730893249441, -11.32770624981968588 ) ) ;
#4226 = ORIENTED_EDGE ( 'NONE', *, *, #7570, .F. ) ;
#4227 = STYLED_ITEM ( 'NONE', ( #5072 ), #7906 ) ;
#4228 = CYLINDRICAL_SURFACE ( 'NONE', #20218, 7.500000000000000000 ) ;
#4229 = CARTESIAN_POINT ( 'NONE',  ( -10.46442989202483709, 10.46442989454075168, 6.587833081519073986 ) ) ;
#4230 = EDGE_CURVE ( 'NONE', #8697, #4546, #10518, .T. ) ;
#4231 = DIRECTION ( 'NONE',  ( -1.000000000000000000, 0.000000000000000000, 0.000000000000000000 ) ) ;
#4232 = VECTOR ( 'NONE', #13666, 1000.000000000000000 ) ;
#4233 = VERTEX_POINT ( 'NONE', #14454 ) ;
#4234 = CARTESIAN_POINT ( 'NONE',  ( 1.660531772554323604, -3.660093687634888848, -2.106514470958295182E-14 ) ) ;
#4235 = CARTESIAN_POINT ( 'NONE',  ( 0.000000000000000000, 63.48283426024851650, 33.96954156735390740 ) ) ;
#4236 = DIRECTION ( 'NONE',  ( 0.000000000000000000, 0.000000000000000000, -1.000000000000000000 ) ) ;
#4237 = ORIENTED_EDGE ( 'NONE', *, *, #11804, .F. ) ;
#4238 = DIRECTION ( 'NONE',  ( 0.000000000000000000, -0.000000000000000000, 1.000000000000000000 ) ) ;
#4239 = ORIENTED_EDGE ( 'NONE', *, *, #38, .T. ) ;
#4240 = DIRECTION ( 'NONE',  ( -1.508455196501572169E-16, 1.000000000000000000, 0.000000000000000000 ) ) ;
#4241 = DIRECTION ( 'NONE',  ( -1.000000000000000000, -0.000000000000000000, -0.000000000000000000 ) ) ;
#4242 = ORIENTED_EDGE ( 'NONE', *, *, #18942, .F. ) ;
#4243 = ORIENTED_EDGE ( 'NONE', *, *, #6100, .F. ) ;
#4244 = PRODUCT_DEFINITION_FORMATION_WITH_SPECIFIED_SOURCE ( 'ANY', '', #7468, .NOT_KNOWN. ) ;
#4245 = CARTESIAN_POINT ( 'NONE',  ( 6.177131623262577698, 0.000000000000000000, 0.000000000000000000 ) ) ;
#4246 = SURFACE_STYLE_FILL_AREA ( #20248 ) ;
#4247 = FACE_BOUND ( 'NONE', #19517, .T. ) ;
#4248 = CIRCLE ( 'NONE', #7278, 2.500000000000002220 ) ;
#4249 = DIRECTION ( 'NONE',  ( 0.000000000000000000, 0.000000000000000000, 1.000000000000000000 ) ) ;
#4250 = CARTESIAN_POINT ( 'NONE',  ( -1.491842756249031510, -7.499999999820660790, -15.82541874981969343 ) ) ;
#4251 = ADVANCED_FACE ( 'NONE', ( #4474 ), #1210, .T. ) ;
#4252 = DIRECTION ( 'NONE',  ( -1.000000000000000000, 0.000000000000000000, 0.000000000000000000 ) ) ;
#4253 = DIRECTION ( 'NONE',  ( -1.000000000000000000, 0.000000000000000000, 0.000000000000000000 ) ) ;
#4254 = PLANE ( 'NONE',  #1885 ) ;
#4255 = ORIENTED_EDGE ( 'NONE', *, *, #5061, .F. ) ;
#4256 = DIRECTION ( 'NONE',  ( 1.000000000000000000, 0.000000000000000000, 0.000000000000000000 ) ) ;
#4257 = AXIS2_PLACEMENT_3D ( 'NONE', #14702, #173, #16386 ) ;
#4258 = EDGE_LOOP ( 'NONE', ( #5088, #8970, #5031, #681 ) ) ;
#4259 = CARTESIAN_POINT ( 'NONE',  ( 3.580422610670020322, -18.00000000043041126, -23.65933124981968660 ) ) ;
#4260 = CARTESIAN_POINT ( 'NONE',  ( 17.61872475889258993, -12.39310755016576948, 75.38263485905284256 ) ) ;
#4261 = ORIENTED_EDGE ( 'NONE', *, *, #1854, .F. ) ;
#4262 = ADVANCED_FACE ( 'NONE', ( #14347, #12536, #10943, #17421 ), #14032, .F. ) ;
#4263 = CARTESIAN_POINT ( 'NONE',  ( 19.99999999999999645, 64.44931368725519860, 10.18420179740629727 ) ) ;
#4264 = ORIENTED_EDGE ( 'NONE', *, *, #17633, .F. ) ;
#4265 = AXIS2_PLACEMENT_3D ( 'NONE', #14019, #2772, #8073 ) ;
#4266 = PRODUCT_DEFINITION_SHAPE ( 'NONE', 'NONE',  #20944 ) ;
#4267 = CARTESIAN_POINT ( 'NONE',  ( 0.000000000000000000, 0.000000000000000000, 43.00000000000000000 ) ) ;
#4268 = DIRECTION ( 'NONE',  ( 0.000000000000000000, 0.000000000000000000, 1.000000000000000000 ) ) ;
#4269 = CARTESIAN_POINT ( 'NONE',  ( -65.00002539999999840, 9.184850993605147944E-16, 7.500000000000000000 ) ) ;
#4270 = ORIENTED_EDGE ( 'NONE', *, *, #20114, .T. ) ;
#4271 = CARTESIAN_POINT ( 'NONE',  ( 19.99999999999999645, 49.77519642624007901, 42.18840861821802690 ) ) ;
#4272 = LINE ( 'NONE', #10949, #13822 ) ;
#4273 = DIRECTION ( 'NONE',  ( 0.000000000000000000, 0.000000000000000000, -1.000000000000000000 ) ) ;
#4274 = CARTESIAN_POINT ( 'NONE',  ( -31.74999999999995737, 0.000000000000000000, 0.000000000000000000 ) ) ;
#4275 = EDGE_CURVE ( 'NONE', #14705, #6265, #15818, .T. ) ;
#4276 = AXIS2_PLACEMENT_3D ( 'NONE', #13169, #1638, #3609 ) ;
#4277 = FACE_OUTER_BOUND ( 'NONE', #7762, .T. ) ;
#4278 = EDGE_LOOP ( 'NONE', ( #14531, #10386 ) ) ;
#4279 = AXIS2_PLACEMENT_3D ( 'NONE', #7781, #12674, #14055 ) ;
#4280 = DIRECTION ( 'NONE',  ( -1.000000000000000000, 0.000000000000000000, -0.000000000000000000 ) ) ;
#4281 = AXIS2_PLACEMENT_3D ( 'NONE', #2771, #7752, #12315 ) ;
#4282 = DIRECTION ( 'NONE',  ( -1.000000000000000000, -0.000000000000000000, -0.000000000000000000 ) ) ;
#4283 = VERTEX_POINT ( 'NONE', #11052 ) ;
#4284 = CARTESIAN_POINT ( 'NONE',  ( 0.000000000000000000, 0.000000000000000000, 0.000000000000000000 ) ) ;
#4285 = DIRECTION ( 'NONE',  ( -1.000000000000000000, 0.000000000000000000, -0.000000000000000000 ) ) ;
#4286 = ORIENTED_EDGE ( 'NONE', *, *, #8961, .F. ) ;
#4287 = CARTESIAN_POINT ( 'NONE',  ( -16.62983158603122291, -6.888301780572501087, -19.69301249981969093 ) ) ;
#4288 = AXIS2_PLACEMENT_3D ( 'NONE', #15260, #12093, #4124 ) ;
#4289 = CARTESIAN_POINT ( 'NONE',  ( 6.177131623262577698, 0.000000000000000000, 0.000000000000000000 ) ) ;
#4290 = CARTESIAN_POINT ( 'NONE',  ( 0.000000000000000000, 0.000000000000000000, -43.00000000000000000 ) ) ;
#4291 = ORIENTED_EDGE ( 'NONE', *, *, #12075, .F. ) ;
#4292 = EDGE_CURVE ( 'NONE', #7789, #9697, #17529, .T. ) ;
#4293 = DIRECTION ( 'NONE',  ( -1.000000000000000000, -0.000000000000000000, 0.000000000000000000 ) ) ;
#4294 = CIRCLE ( 'NONE', #4972, 40.00000000000000000 ) ;
#4295 = ORIENTED_EDGE ( 'NONE', *, *, #9485, .F. ) ;
#4296 = CARTESIAN_POINT ( 'NONE',  ( 19.99999999999999645, 0.000000000000000000, 0.000000000000000000 ) ) ;
#4297 = AXIS2_PLACEMENT_3D ( 'NONE', #14532, #13350, #17916 ) ;
#4298 = ADVANCED_FACE ( 'NONE', ( #1414, #1633 ), #16236, .T. ) ;
#4299 = ORIENTED_EDGE ( 'NONE', *, *, #13558, .F. ) ;
#4300 = CIRCLE ( 'NONE', #8689, 18.00000000000000000 ) ;
#4301 = ADVANCED_FACE ( 'NONE', ( #2024 ), #19514, .T. ) ;
#4302 = EDGE_CURVE ( 'NONE', #2621, #12626, #15931, .T. ) ;
#4303 = CARTESIAN_POINT ( 'NONE',  ( 31.43473485066228079, -112.4512879816791013, 74.54413784199456927 ) ) ;
#4304 = B_SPLINE_CURVE_WITH_KNOTS ( 'NONE', 3,
 ( #12665, #20493, #19125, #14246, #20597, #9372 ),
 .UNSPECIFIED., .F., .F.,
 ( 4, 2, 4 ),
 ( 0.002336974151641539946, 0.003500975885716448889, 0.004664977619791357832 ),
 .UNSPECIFIED. ) ;
#4305 = DIRECTION ( 'NONE',  ( 0.000000000000000000, 0.000000000000000000, -1.000000000000000000 ) ) ;
#4306 = CONTEXT_DEPENDENT_SHAPE_REPRESENTATION ( #13877, #19808 ) ;
#4307 = CARTESIAN_POINT ( 'NONE',  ( 8.382925368423272516, -12.54593441764187745, -1.637051831158454984 ) ) ;
#4308 = ORIENTED_EDGE ( 'NONE', *, *, #4497, .F. ) ;
#4309 = VECTOR ( 'NONE', #13528, 1000.000000000000000 ) ;
#4310 = DIRECTION ( 'NONE',  ( 0.000000000000000000, 0.000000000000000000, -1.000000000000000000 ) ) ;
#4311 = ORIENTED_EDGE ( 'NONE', *, *, #6011, .F. ) ;
#4312 = DIRECTION ( 'NONE',  ( 0.000000000000000000, 0.000000000000000000, 1.000000000000000000 ) ) ;
#4313 = EDGE_CURVE ( 'NONE', #18213, #20933, #16332, .T. ) ;
#4314 = VECTOR ( 'NONE', #14203, 1000.000000000000000 ) ;
#4315 = CARTESIAN_POINT ( 'NONE',  ( 16.62983158437509346, -6.888301784570737496, 12.56801250018031091 ) ) ;
#4316 = CIRCLE ( 'NONE', #931, 0.3200000000000008393 ) ;
#4317 = DIRECTION ( 'NONE',  ( -0.000000000000000000, -0.000000000000000000, -1.000000000000000000 ) ) ;
#4318 = DIRECTION ( 'NONE',  ( -1.000000000000000000, 0.000000000000000000, 0.000000000000000000 ) ) ;
#4319 = ORIENTED_EDGE ( 'NONE', *, *, #20509, .F. ) ;
#4320 = EDGE_CURVE ( 'NONE', #6274, #17007, #328, .T. ) ;
#4321 = CARTESIAN_POINT ( 'NONE',  ( 19.99999999999999645, 0.000000000000000000, 0.000000000000000000 ) ) ;
#4322 = DIRECTION ( 'NONE',  ( -1.000000000000000000, 0.000000000000000000, 0.000000000000000000 ) ) ;
#4323 = ORIENTED_EDGE ( 'NONE', *, *, #6615, .F. ) ;
#4324 = CARTESIAN_POINT ( 'NONE',  ( 10.68115262102694807, -20.37288806868372149, -76.58146718639416406 ) ) ;
#4325 = LINE ( 'NONE', #17255, #12391 ) ;
#4326 = EDGE_CURVE ( 'NONE', #6250, #1069, #5197, .T. ) ;
#4327 = CARTESIAN_POINT ( 'NONE',  ( 6.888301780572505528, -16.62983158603121581, -14.52886249981968980 ) ) ;
#4328 = VECTOR ( 'NONE', #9898, 1000.000000000000000 ) ;
#4329 = ORIENTED_EDGE ( 'NONE', *, *, #2538, .F. ) ;
#4330 = DIRECTION ( 'NONE',  ( 0.000000000000000000, 0.000000000000000000, 1.000000000000000000 ) ) ;
#4331 = AXIS2_PLACEMENT_3D ( 'NONE', #13440, #5151, #5053 ) ;
#4332 = CYLINDRICAL_SURFACE ( 'NONE', #19016, 27.60000000002759890 ) ;
#4333 = FACE_BOUND ( 'NONE', #8946, .T. ) ;
#4334 = CARTESIAN_POINT ( 'NONE',  ( 23.13963350654227824, -26.35784117651622793, -120.0000000000000142 ) ) ;
#4335 = DIRECTION ( 'NONE',  ( 3.374236624099838250E-32, -1.836909530733573776E-16, -1.000000000000000000 ) ) ;
#4336 = CARTESIAN_POINT ( 'NONE',  ( 16.62983158437509701, -6.888301784570740161, 5.047612500180310491 ) ) ;
#4337 = UNCERTAINTY_MEASURE_WITH_UNIT (LENGTH_MEASURE( 1.000000000000000082E-05 ), #4024, 'distance_accuracy_value', 'NONE');
#4338 = DIRECTION ( 'NONE',  ( -0.000000000000000000, -0.000000000000000000, 1.000000000000000000 ) ) ;
#4339 = EDGE_LOOP ( 'NONE', ( #8825, #6400, #4631, #13400 ) ) ;
#4340 = DIRECTION ( 'NONE',  ( -0.000000000000000000, -0.000000000000000000, -1.000000000000000000 ) ) ;
#4341 = EDGE_CURVE ( 'NONE', #8208, #9811, #9174, .T. ) ;
#4342 = CARTESIAN_POINT ( 'NONE',  ( -14.79893867758296544, 1.779018419858780125E-09, 5.409708081519076117 ) ) ;
#4343 = CARTESIAN_POINT ( 'NONE',  ( -6.232800000000000118, 9.267171751443831555E-16, -7.567219999999999835 ) ) ;
#4344 = ORIENTED_EDGE ( 'NONE', *, *, #132, .F. ) ;
#4345 = CARTESIAN_POINT ( 'NONE',  ( 24.99999999999999645, -99.99999999999998579, -52.00000000000000000 ) ) ;
#4346 = CARTESIAN_POINT ( 'NONE',  ( 10.19618095047497874, -15.25966317163203279, -22.34379374981968880 ) ) ;
#4347 = CARTESIAN_POINT ( 'NONE',  ( 19.99999999999999645, 0.000000000000000000, 0.000000000000000000 ) ) ;
#4348 = ORIENTED_EDGE ( 'NONE', *, *, #2365, .F. ) ;
#4349 = DIRECTION ( 'NONE',  ( 0.000000000000000000, -0.8169698930104356549, -0.5766803221148764091 ) ) ;
#4350 = ORIENTED_EDGE ( 'NONE', *, *, #17358, .T. ) ;
#4351 = CARTESIAN_POINT ( 'NONE',  ( 2.500000000000000000, 2.500728763858895382E-16, -2.041999999999999815 ) ) ;
#4352 = DIRECTION ( 'NONE',  ( -1.000000000000000000, -0.000000000000000000, -0.000000000000000000 ) ) ;
#4353 = ORIENTED_EDGE ( 'NONE', *, *, #19178, .F. ) ;
#4354 = ORIENTED_EDGE ( 'NONE', *, *, #13484, .T. ) ;
#4355 = CARTESIAN_POINT ( 'NONE',  ( 4.000000000000003553, 2.309401076758480720, -5.599999999999999645 ) ) ;
#4356 = EDGE_CURVE ( 'NONE', #18180, #6701, #11253, .T. ) ;
#4357 = FILL_AREA_STYLE_COLOUR ( '', #16152 ) ;
#4358 = LINE ( 'NONE', #9442, #15349 ) ;
#4359 = CARTESIAN_POINT ( 'NONE',  ( 50.00000000000000000, -124.9999999999999858, 90.00000000000001421 ) ) ;
#4360 = CARTESIAN_POINT ( 'NONE',  ( 6.358192987158590270, -4.248408730893245000, -27.01760624981969272 ) ) ;
#4361 = CARTESIAN_POINT ( 'NONE',  ( 9.999999999999998224, -46.17500197033020015, -55.24372537266445704 ) ) ;
#4362 = DIRECTION ( 'NONE',  ( 0.000000000000000000, 0.000000000000000000, 1.000000000000000000 ) ) ;
#4363 = DIRECTION ( 'NONE',  ( -1.000000000000000000, 0.000000000000000000, -0.000000000000000000 ) ) ;
#4364 = ORIENTED_EDGE ( 'NONE', *, *, #6372, .T. ) ;
#4365 = FACE_OUTER_BOUND ( 'NONE', #19281, .T. ) ;
#4366 = ORIENTED_EDGE ( 'NONE', *, *, #9307, .F. ) ;
#4367 = CARTESIAN_POINT ( 'NONE',  ( -15.25966317163203279, -10.19618095047498052, -12.46714374981968909 ) ) ;
#4368 = DIRECTION ( 'NONE',  ( 1.000000000000000000, -0.000000000000000000, -0.000000000000000000 ) ) ;
#4369 = ORIENTED_EDGE ( 'NONE', *, *, #5087, .F. ) ;
#4370 = DIRECTION ( 'NONE',  ( 0.000000000000000000, 0.3984010898462422845, -0.9172113015054527141 ) ) ;
#4371 = ORIENTED_EDGE ( 'NONE', *, *, #12460, .T. ) ;
#4372 = DIRECTION ( 'NONE',  ( -1.000000000000000000, -0.000000000000000000, -0.000000000000000000 ) ) ;
#4373 = DIRECTION ( 'NONE',  ( 0.000000000000000000, 0.000000000000000000, 1.000000000000000000 ) ) ;
#4374 = DIRECTION ( 'NONE',  ( 0.000000000000000000, -0.7308359642781302457, 0.6825531432186475733 ) ) ;
#4375 = EDGE_LOOP ( 'NONE', ( #5203, #17782, #16517, #14685 ) ) ;
#4376 = DIRECTION ( 'NONE',  ( 1.000000000000000000, 0.000000000000000000, 0.000000000000000000 ) ) ;
#4377 = ADVANCED_FACE ( 'NONE', ( #19613 ), #1749, .T. ) ;
#4378 = CARTESIAN_POINT ( 'NONE',  ( 5.000000000000000888, 4.250000000000000000, 0.000000000000000000 ) ) ;
#4379 = DIRECTION ( 'NONE',  ( -1.000000000000000000, 0.000000000000000000, 0.000000000000000000 ) ) ;
#4380 = DIRECTION ( 'NONE',  ( -0.000000000000000000, -0.000000000000000000, 1.000000000000000000 ) ) ;
#4381 = FACE_OUTER_BOUND ( 'NONE', #14061, .T. ) ;
#4382 = ORIENTED_EDGE ( 'NONE', *, *, #4753, .F. ) ;
#4383 = CARTESIAN_POINT ( 'NONE',  ( 19.99999999999999645, -65.23577793412346182, 1.313498510941474740 ) ) ;
#4384 = LINE ( 'NONE', #20496, #7447 ) ;
#4385 = ORIENTED_EDGE ( 'NONE', *, *, #15915, .T. ) ;
#4386 = CYLINDRICAL_SURFACE ( 'NONE', #12999, 2.649999999999994582 ) ;
#4387 = LINE ( 'NONE', #17438, #14334 ) ;
#4388 = VERTEX_POINT ( 'NONE', #6781 ) ;
#4389 = CARTESIAN_POINT ( 'NONE',  ( 6.888301780572507305, -16.62983158603121936, -22.04926249981969022 ) ) ;
#4390 = CARTESIAN_POINT ( 'NONE',  ( 150.0000507999999968, 0.000000000000000000, 0.000000000000000000 ) ) ;
#4391 = DIRECTION ( 'NONE',  ( 1.000000000000000000, 0.000000000000000000, 0.000000000000000000 ) ) ;
#4392 = SHAPE_REPRESENTATION ( 'Sealed Cast Iron Gearbox Casing', ( #12461 ), #2940 ) ;
#4393 = EDGE_LOOP ( 'NONE', ( #9013, #20128 ) ) ;
#4394 = DIRECTION ( 'NONE',  ( -1.000000000000000000, 0.000000000000000000, -0.000000000000000000 ) ) ;
#4395 = ORIENTED_EDGE ( 'NONE', *, *, #1946, .T. ) ;
#4396 = DIRECTION ( 'NONE',  ( 0.000000000000000000, 0.8169698930104392076, 0.5766803221148710801 ) ) ;
#4397 = ORIENTED_EDGE ( 'NONE', *, *, #10568, .F. ) ;
#4398 = VECTOR ( 'NONE', #9473, 1000.000000000000000 ) ;
#4399 = APPLICATION_CONTEXT ( 'automotive_design' ) ;
#4400 = DIRECTION ( 'NONE',  ( -1.000000000000000000, -0.000000000000000000, -0.000000000000000000 ) ) ;
#4401 = DIRECTION ( 'NONE',  ( 0.000000000000000000, 0.000000000000000000, -1.000000000000000000 ) ) ;
#4402 = CONTEXT_DEPENDENT_SHAPE_REPRESENTATION ( #4108, #16775 ) ;
#4403 = CARTESIAN_POINT ( 'NONE',  ( -2.943691925285397470, 14.79893867793684059, 3.664510668841544305 ) ) ;
#4404 = EDGE_CURVE ( 'NONE', #7823, #16612, #10879, .T. ) ;
#4405 = ORIENTED_EDGE ( 'NONE', *, *, #13384, .T. ) ;
#4406 = EDGE_CURVE ( 'NONE', #13080, #16803, #11666, .T. ) ;
#4407 = CARTESIAN_POINT ( 'NONE',  ( -30.00000000000000000, -151.4095880458873467, 44.60680010464249534 ) ) ;
#4408 = ORIENTED_EDGE ( 'NONE', *, *, #5089, .T. ) ;
#4409 = CARTESIAN_POINT ( 'NONE',  ( -3.612956115288154635, -21.20621163160360112, 76.17826316794804598 ) ) ;
#4410 = CARTESIAN_POINT ( 'NONE',  ( 15.25966317163202568, 10.19618095047498230, 11.09535625018031091 ) ) ;
#4411 = CARTESIAN_POINT ( 'NONE',  ( 2.500000000000000000, 0.000000000000000000, 0.000000000000000000 ) ) ;
#4412 = CIRCLE ( 'NONE', #19968, 72.00000000007199219 ) ;
#4413 = CARTESIAN_POINT ( 'NONE',  ( -12.50000000000000533, 0.000000000000000000, 43.00000000000000000 ) ) ;
#4414 = EDGE_CURVE ( 'NONE', #10695, #12643, #9185, .T. ) ;
#4415 = ORIENTED_EDGE ( 'NONE', *, *, #11009, .T. ) ;
#4416 = CARTESIAN_POINT ( 'NONE',  ( -24.99999999999999289, -113.2094389508847314, 74.86138894033631175 ) ) ;
#4417 = CYLINDRICAL_SURFACE ( 'NONE', #17190, 3.199999999999994404 ) ;
#4418 = VECTOR ( 'NONE', #11120, 1000.000000000000000 ) ;
#4419 = ORIENTED_EDGE ( 'NONE', *, *, #14792, .T. ) ;
#4420 = LINE ( 'NONE', #7383, #15658 ) ;
#4421 = CARTESIAN_POINT ( 'NONE',  ( 7.500000000000000888, 4.207617034106124418E-15, 0.3738000000023073421 ) ) ;
#4422 = CARTESIAN_POINT ( 'NONE',  ( 17.99999999956957808, -3.580422614997675446, -6.576518749819692644 ) ) ;
#4423 = ORIENTED_EDGE ( 'NONE', *, *, #19718, .F. ) ;
#4424 = DIRECTION ( 'NONE',  ( -1.000000000000000000, -0.000000000000000000, -0.000000000000000000 ) ) ;
#4425 = ADVANCED_FACE ( 'NONE', ( #3605 ), #3310, .T. ) ;
#4426 = DIRECTION ( 'NONE',  ( 0.000000000000000000, 0.000000000000000000, 1.000000000000000000 ) ) ;
#4427 = CIRCLE ( 'NONE', #10171, 27.60000000002759890 ) ;
#4428 = CYLINDRICAL_SURFACE ( 'NONE', #11238, 7.500000000000000000 ) ;
#4429 = CARTESIAN_POINT ( 'NONE',  ( -4.000000000000000000, 0.000000000000000000, -5.599999999999999645 ) ) ;
#4430 = DIRECTION ( 'NONE',  ( 0.000000000000000000, 0.000000000000000000, -1.000000000000000000 ) ) ;
#4431 = CARTESIAN_POINT ( 'NONE',  ( 6.888301784570730391, 16.62983158437510411, 12.11636250018031014 ) ) ;
#4432 = EDGE_CURVE ( 'NONE', #1628, #6474, #374, .T. ) ;
#4433 = EDGE_CURVE ( 'NONE', #440, #896, #5448, .T. ) ;
#4434 = CARTESIAN_POINT ( 'NONE',  ( 4.248408729364579806, -6.358192988180021210, -20.16364374981968766 ) ) ;
#4435 = AXIS2_PLACEMENT_3D ( 'NONE', #3727, #5740, #8812 ) ;
#4436 = ORIENTED_EDGE ( 'NONE', *, *, #6100, .T. ) ;
#4437 = DIRECTION ( 'NONE',  ( -1.000000000000000000, -0.000000000000000000, 0.000000000000000000 ) ) ;
#4438 = CARTESIAN_POINT ( 'NONE',  ( -14.79893867793683349, -2.943691925285398359, 14.54017683151907647 ) ) ;
#4439 = EDGE_CURVE ( 'NONE', #16465, #7909, #10082, .T. ) ;
#4440 = ORIENTED_EDGE ( 'NONE', *, *, #10028, .T. ) ;
#4441 = CARTESIAN_POINT ( 'NONE',  ( 0.000000000000000000, 0.000000000000000000, 0.000000000000000000 ) ) ;
#4442 = CARTESIAN_POINT ( 'NONE',  ( -18.00000000000000000, 2.163826221265758884E-09, -19.10394999981969022 ) ) ;
#4443 = DIRECTION ( 'NONE',  ( 0.000000000000000000, 0.000000000000000000, -1.000000000000000000 ) ) ;
#4444 = VERTEX_POINT ( 'NONE', #1921 ) ;
#4445 = CARTESIAN_POINT ( 'NONE',  ( 0.000000000000000000, 0.000000000000000000, 0.000000000000000000 ) ) ;
#4446 = ORIENTED_EDGE ( 'NONE', *, *, #986, .F. ) ;
#4447 = CARTESIAN_POINT ( 'NONE',  ( 40.91005719111474548, -14.31667062835577120, -80.10683058186114636 ) ) ;
#4448 = CARTESIAN_POINT ( 'NONE',  ( 0.000000000000000000, 0.000000000000000000, 0.000000000000000000 ) ) ;
#4449 = VERTEX_POINT ( 'NONE', #11466 ) ;
#4450 = CIRCLE ( 'NONE', #17317, 2.099999999999990763 ) ;
#4451 = VERTEX_POINT ( 'NONE', #437 ) ;
#4452 = CARTESIAN_POINT ( 'NONE',  ( 49.35000000000000142, -39.99999999999999289, 5.000000000000000000 ) ) ;
#4453 = EDGE_CURVE ( 'NONE', #4018, #1116, #8381, .T. ) ;
#4454 = AXIS2_PLACEMENT_3D ( 'NONE', #11035, #17514, #2985 ) ;
#4455 = DIRECTION ( 'NONE',  ( 0.000000000000000000, 0.000000000000000000, 1.000000000000000000 ) ) ;
#4456 = EDGE_CURVE ( 'NONE', #2016, #5196, #8173, .T. ) ;
#4457 = DIRECTION ( 'NONE',  ( -1.000000000000000000, 0.000000000000000000, 0.000000000000000000 ) ) ;
#4458 = CIRCLE ( 'NONE', #15637, 27.60000000002759890 ) ;
#4459 = AXIS2_PLACEMENT_3D ( 'NONE', #17643, #6396, #6294 ) ;
#4460 = CARTESIAN_POINT ( 'NONE',  ( 1.491842754445842134, -7.500000000179339210, -16.41448124981968704 ) ) ;
#4461 = FACE_OUTER_BOUND ( 'NONE', #13655, .T. ) ;
#4462 = VECTOR ( 'NONE', #1698, 1000.000000000000000 ) ;
#4463 = DIRECTION ( 'NONE',  ( -1.000000000000000000, 0.000000000000000000, 0.000000000000000000 ) ) ;
#4464 = DIRECTION ( 'NONE',  ( 0.000000000000000000, -1.000000000000000000, 0.000000000000000000 ) ) ;
#4465 = EDGE_LOOP ( 'NONE', ( #1723, #19275, #11473, #11086 ) ) ;
#4466 = CARTESIAN_POINT ( 'NONE',  ( -8.999999999999987566, -85.00000000000000000, 0.000000000000000000 ) ) ;
#4467 = VERTEX_POINT ( 'NONE', #13571 ) ;
#4468 = CARTESIAN_POINT ( 'NONE',  ( -10.19618095414378622, -15.25966316918061416, -13.05620624981969158 ) ) ;
#4469 = CYLINDRICAL_SURFACE ( 'NONE', #9959, 55.00000000000000711 ) ;
#4470 = PRESENTATION_LAYER_ASSIGNMENT (  '', '', ( #12939 ) ) ;
#4471 = VERTEX_POINT ( 'NONE', #745 ) ;
#4472 = DIRECTION ( 'NONE',  ( -1.000000000000000000, -0.000000000000000000, 0.000000000000000000 ) ) ;
#4473 = ORIENTED_EDGE ( 'NONE', *, *, #14171, .F. ) ;
#4474 = FACE_OUTER_BOUND ( 'NONE', #17581, .T. ) ;
#4475 = DIRECTION ( 'NONE',  ( 0.000000000000000000, 0.000000000000000000, 1.000000000000000000 ) ) ;
#4476 = CARTESIAN_POINT ( 'NONE',  ( 19.99999999999999645, -19.38316218894168586, -61.87375713201008409 ) ) ;
#4477 = ORIENTED_EDGE ( 'NONE', *, *, #8889, .F. ) ;
#4478 = DIRECTION ( 'NONE',  ( 0.000000000000000000, -0.8169698930104469792, 0.5766803221148600889 ) ) ;
#4479 = VECTOR ( 'NONE', #8564, 1000.000000000000000 ) ;
#4480 = CIRCLE ( 'NONE', #11585, 11.17999999999999261 ) ;
#4481 = AXIS2_PLACEMENT_3D ( 'NONE', #2305, #8650, #15128 ) ;
#4482 = VECTOR ( 'NONE', #8248, 1000.000000000000000 ) ;
#4483 = DIRECTION ( 'NONE',  ( 1.000000000000000000, -1.387778780781445676E-15, 0.000000000000000000 ) ) ;
#4484 = CARTESIAN_POINT ( 'NONE',  ( 10.19618095047497697, -15.25966317163202923, -24.24839374981969087 ) ) ;
#4485 = DIRECTION ( 'NONE',  ( 1.000000000000000000, 0.000000000000000000, 0.000000000000000000 ) ) ;
#4486 = DIRECTION ( 'NONE',  ( 0.000000000000000000, 0.000000000000000000, 1.000000000000000000 ) ) ;
#4487 = VERTEX_POINT ( 'NONE', #2335 ) ;
#4488 = CARTESIAN_POINT ( 'NONE',  ( 85.00002539999999840, 3.872983346207417021, 1.000000000000000000 ) ) ;
#4489 = DIRECTION ( 'NONE',  ( 0.000000000000000000, 0.000000000000000000, 1.000000000000000000 ) ) ;
#4490 = ORIENTED_EDGE ( 'NONE', *, *, #13743, .T. ) ;
#4491 = AXIS2_PLACEMENT_3D ( 'NONE', #15325, #16914, #7369 ) ;
#4492 = DIRECTION ( 'NONE',  ( -1.000000000000000000, 0.000000000000000000, 0.000000000000000000 ) ) ;
#4493 = DIRECTION ( 'NONE',  ( 0.000000000000000000, 0.000000000000000000, 1.000000000000000000 ) ) ;
#4494 = EDGE_CURVE ( 'NONE', #10263, #18180, #8823, .T. ) ;
#4495 = AXIS2_PLACEMENT_3D ( 'NONE', #14166, #14259, #7891 ) ;
#4496 = ORIENTED_EDGE ( 'NONE', *, *, #12465, .F. ) ;
#4497 = EDGE_CURVE ( 'NONE', #17002, #19648, #4450, .T. ) ;
#4498 = CARTESIAN_POINT ( 'NONE',  ( 3.580422614997668340, 17.99999999956958519, -7.028168749819689864 ) ) ;
#4499 = CIRCLE ( 'NONE', #11590, 7.500000000000000000 ) ;
#4500 = CARTESIAN_POINT ( 'NONE',  ( 5.000000000000002665, 0.000000000000000000, -2.700000000000000622 ) ) ;
#4501 = DIRECTION ( 'NONE',  ( -0.000000000000000000, -0.000000000000000000, 1.000000000000000000 ) ) ;
#4502 = EDGE_LOOP ( 'NONE', ( #8785, #12717, #8454, #3807 ) ) ;
#4503 = CARTESIAN_POINT ( 'NONE',  ( 9.470358143689555419, -1.138454911109683768E-09, 36.10922829754954932 ) ) ;
#4504 = VERTEX_POINT ( 'NONE', #15061 ) ;
#4505 = LINE ( 'NONE', #4717, #4113 ) ;
#4506 = AXIS2_PLACEMENT_3D ( 'NONE', #9904, #11399, #4726 ) ;
#4507 = CARTESIAN_POINT ( 'NONE',  ( 3.999999999999990674, -2.309401076758548221, -5.242734410091827613 ) ) ;
#4508 = AXIS2_PLACEMENT_3D ( 'NONE', #11490, #477, #14883 ) ;
#4509 = DIRECTION ( 'NONE',  ( 0.000000000000000000, 0.000000000000000000, 1.000000000000000000 ) ) ;
#4510 = ITEM_DEFINED_TRANSFORMATION ( 'NONE', 'NONE', #19142,  #12461 ) ;
#4511 = EDGE_CURVE ( 'NONE', #16270, #2251, #10191, .T. ) ;
#4512 = CARTESIAN_POINT ( 'NONE',  ( 5.663308646854342321, -13.67243654778935635, -10.76752058115845223 ) ) ;
#4513 = ORIENTED_EDGE ( 'NONE', *, *, #3743, .T. ) ;
#4514 = FACE_BOUND ( 'NONE', #18203, .T. ) ;
#4515 = LINE ( 'NONE', #17458, #11265 ) ;
#4516 = ORIENTED_EDGE ( 'NONE', *, *, #14170, .F. ) ;
#4517 =( BOUNDED_CURVE ( )  B_SPLINE_CURVE ( 2, ( #19040, #10980, #2929, #15859, #8011, #1352, #7796, #14270, #12690, #15952, #1454, #19147, #14492, #4621, #11093, #17566, #20931 ),
 .UNSPECIFIED., .F., .T. ) 
 B_SPLINE_CURVE_WITH_KNOTS ( ( 3, 2, 2, 2, 2, 2, 2, 2, 3 ),
 ( 0.7000000000038510972, 0.7125000000038511638, 0.7250000000038511194, 0.7375000000038511860, 0.7500000000038511416, 0.7625000000038510972, 0.7750000000038511638, 0.7875000000038511194, 0.8000000000038511860 ),
 .UNSPECIFIED. ) 
 CURVE ( )  GEOMETRIC_REPRESENTATION_ITEM ( )  RATIONAL_B_SPLINE_CURVE ( ( 0.9999999999940800688, 0.9807852804091503618, 1.000000000000000000, 0.9807852804032304306, 1.000000000000000000, 0.9807852804032304306, 1.000000000000000000, 0.9807852804032304306, 1.000000000000000000, 0.9807852804032304306, 1.000000000000000000, 0.9807852804032304306, 1.000000000000000000, 0.9807852804032304306, 1.000000000000000000, 0.9807852803973104994, 1.000000000005919931 ) ) 
 REPRESENTATION_ITEM ( '' )  );
#4518 = AXIS2_PLACEMENT_3D ( 'NONE', #8355, #3578, #11445 ) ;
#4519 = CARTESIAN_POINT ( 'NONE',  ( 11.40258492152624115, -18.23049771964689825, 77.70848679321215968 ) ) ;
#4520 = CARTESIAN_POINT ( 'NONE',  ( -17.99999999999999645, 2.163826221265758470E-09, 7.266450000180311619 ) ) ;
#4521 = FACE_OUTER_BOUND ( 'NONE', #18629, .T. ) ;
#4522 = PLANE ( 'NONE',  #14453 ) ;
#4523 = AXIS2_PLACEMENT_3D ( 'NONE', #16441, #1930, #10503 ) ;
#4524 = ORIENTED_EDGE ( 'NONE', *, *, #7812, .T. ) ;
#4525 = FACE_OUTER_BOUND ( 'NONE', #9708, .T. ) ;
#4526 = DIRECTION ( 'NONE',  ( 1.000000000000000000, 0.000000000000000000, 0.000000000000000000 ) ) ;
#4527 = ORIENTED_EDGE ( 'NONE', *, *, #12542, .F. ) ;
#4528 = ADVANCED_FACE ( 'NONE', ( #16860 ), #20242, .T. ) ;
#4529 = DIRECTION ( 'NONE',  ( -1.000000000000000000, -0.000000000000000000, -0.000000000000000000 ) ) ;
#4530 = DIRECTION ( 'NONE',  ( 0.000000000000000000, 0.000000000000000000, -1.000000000000000000 ) ) ;
#4531 = CARTESIAN_POINT ( 'NONE',  ( -18.00000000043040771, -3.580422610670021211, -21.30308124981969442 ) ) ;
#4532 = AXIS2_PLACEMENT_3D ( 'NONE', #16969, #18250, #7011 ) ;
#4533 = VERTEX_POINT ( 'NONE', #7090 ) ;
#4534 = CARTESIAN_POINT ( 'NONE',  ( -4.248408730893249441, -6.358192987158596488, -8.971456249819688367 ) ) ;
#4535 = AXIS2_PLACEMENT_3D ( 'NONE', #16842, #13662, #2109 ) ;
#4536 = FACE_BOUND ( 'NONE', #12063, .T. ) ;
#4537 = CARTESIAN_POINT ( 'NONE',  ( -30.00000000000000000, -85.00000000000000000, -1.040949779275250179E-14 ) ) ;
#4538 = LINE ( 'NONE', #17477, #8883 ) ;
#4539 = EDGE_CURVE ( 'NONE', #13894, #12404, #10608, .T. ) ;
#4540 = DIRECTION ( 'NONE',  ( -7.888609052210117178E-31, 1.577721810442023260E-30, 1.000000000000000000 ) ) ;
#4541 = CARTESIAN_POINT ( 'NONE',  ( 10.19618095047498052, -15.25966317163203456, 5.931206250180308004 ) ) ;
#4542 = AXIS2_PLACEMENT_3D ( 'NONE', #18456, #3923, #10406 ) ;
#4543 = ADVANCED_FACE ( 'NONE', ( #10396 ), #3913, .T. ) ;
#4544 = CIRCLE ( 'NONE', #2165, 65.24900000006525147 ) ;
#4545 = DIRECTION ( 'NONE',  ( 1.000000000000000000, 0.000000000000000000, 0.000000000000000000 ) ) ;
#4546 = VERTEX_POINT ( 'NONE', #5713 ) ;
#4547 = CARTESIAN_POINT ( 'NONE',  ( 3.600000000000060485, 10.82531754730546147, 166.0000000000000000 ) ) ;
#4548 = CARTESIAN_POINT ( 'NONE',  ( 10.46442989202483531, -10.46442989454075168, 11.30033308151907789 ) ) ;
#4549 = CARTESIAN_POINT ( 'NONE',  ( 18.13963350654227469, -26.35784117651622793, -120.0000000000000142 ) ) ;
#4550 = AXIS2_PLACEMENT_3D ( 'NONE', #13171, #17941, #11566 ) ;
#4551 = VERTEX_POINT ( 'NONE', #15482 ) ;
#4552 = DIRECTION ( 'NONE',  ( -1.000000000000000000, 0.000000000000000000, 0.000000000000000000 ) ) ;
#4553 = DIRECTION ( 'NONE',  ( 1.000000000000000000, 0.000000000000000000, 0.000000000000000000 ) ) ;
#4554 = DIRECTION ( 'NONE',  ( -1.000000000000000000, -0.000000000000000000, 0.000000000000000000 ) ) ;
#4555 = ORIENTED_EDGE ( 'NONE', *, *, #17653, .F. ) ;
#4556 = ADVANCED_FACE ( 'NONE', ( #18448 ), #19921, .T. ) ;
#4557 = DIRECTION ( 'NONE',  ( -1.000000000000000000, -0.000000000000000000, -0.000000000000000000 ) ) ;
#4558 = ORIENTED_EDGE ( 'NONE', *, *, #10782, .F. ) ;
#4559 = VECTOR ( 'NONE', #16770, 1000.000000000000000 ) ;
#4560 = DIRECTION ( 'NONE',  ( 1.000000000000000000, 0.000000000000000000, 0.000000000000000000 ) ) ;
#4561 = DIRECTION ( 'NONE',  ( 0.000000000000000000, 0.000000000000000000, 1.000000000000000000 ) ) ;
#4562 = EDGE_CURVE ( 'NONE', #12535, #10231, #14936, .T. ) ;
#4563 = ORIENTED_EDGE ( 'NONE', *, *, #8441, .T. ) ;
#4564 = ORIENTED_EDGE ( 'NONE', *, *, #12360, .T. ) ;
#4565 = CARTESIAN_POINT ( 'NONE',  ( 31.43268490318742181, -112.4462444941460006, -74.54209189151036696 ) ) ;
#4566 = ADVANCED_FACE ( 'NONE', ( #19821 ), #642, .T. ) ;
#4567 =( NAMED_UNIT ( * ) PLANE_ANGLE_UNIT ( ) SI_UNIT ( $, .RADIAN. ) );
#4568 = DIRECTION ( 'NONE',  ( 0.000000000000000000, 0.000000000000000000, -1.000000000000000000 ) ) ;
#4569 = FACE_OUTER_BOUND ( 'NONE', #20072, .T. ) ;
#4570 = CARTESIAN_POINT ( 'NONE',  ( -11.17563879704982988, 2.222972771497744748, -6.775358999352572908 ) ) ;
#4571 = CIRCLE ( 'NONE', #11339, 17.50000000000000355 ) ;
#4572 = CARTESIAN_POINT ( 'NONE',  ( -5.303300859536631329, -5.303300858261583706, -24.36682499981969485 ) ) ;
#4573 = CARTESIAN_POINT ( 'NONE',  ( 2.099999999999999645, 0.000000000000000000, -0.2800830152838832965 ) ) ;
#4574 = ADVANCED_FACE ( 'NONE', ( #11774, #13682 ), #18239, .T. ) ;
#4575 = CARTESIAN_POINT ( 'NONE',  ( -12.50000000000000533, 0.000000000000000000, 46.00000000000000711 ) ) ;
#4576 = DIRECTION ( 'NONE',  ( -0.000000000000000000, -0.000000000000000000, 1.000000000000000000 ) ) ;
#4577 = ADVANCED_FACE ( 'NONE', ( #3704 ), #16640, .F. ) ;
#4578 = ORIENTED_EDGE ( 'NONE', *, *, #10645, .F. ) ;
#4579 = DIRECTION ( 'NONE',  ( -1.000000000000000000, 0.000000000000000000, 0.000000000000000000 ) ) ;
#4580 = ORIENTED_EDGE ( 'NONE', *, *, #10663, .T. ) ;
#4581 = CARTESIAN_POINT ( 'NONE',  ( -6.888301780572501976, 16.62983158603122291, -9.816362499819687670 ) ) ;
#4582 = DIRECTION ( 'NONE',  ( 0.000000000000000000, -0.000000000000000000, 1.000000000000000000 ) ) ;
#4583 = CARTESIAN_POINT ( 'NONE',  ( 17.99999999999999645, -2.163824016901520184E-09, 21.40395000018031268 ) ) ;
#4584 = ORIENTED_EDGE ( 'NONE', *, *, #1345, .F. ) ;
#4585 = CARTESIAN_POINT ( 'NONE',  ( -52.00000000000000000, -99.99999999999998579, 0.000000000000000000 ) ) ;
#4586 = EDGE_LOOP ( 'NONE', ( #5024, #11019, #6160, #16405 ) ) ;
#4587 = DIRECTION ( 'NONE',  ( -1.000000000000000000, 0.000000000000000000, -0.000000000000000000 ) ) ;
#4588 = FACE_OUTER_BOUND ( 'NONE', #4146, .T. ) ;
#4589 = CARTESIAN_POINT ( 'NONE',  ( -5.303300858261584594, 5.303300859536631329, -3.160574999819691477 ) ) ;
#4590 = ADVANCED_FACE ( 'NONE', ( #20129 ), #12579, .T. ) ;
#4591 = ORIENTED_EDGE ( 'NONE', *, *, #13216, .T. ) ;
#4592 = CARTESIAN_POINT ( 'NONE',  ( 19.99999999999999645, 6.872116855663142232, 64.47358224882421496 ) ) ;
#4593 = VECTOR ( 'NONE', #15721, 1000.000000000000114 ) ;
#4594 = LINE ( 'NONE', #5966, #8301 ) ;
#4595 = DIRECTION ( 'NONE',  ( -0.000000000000000000, -0.000000000000000000, 1.000000000000000000 ) ) ;
#4596 = DIRECTION ( 'NONE',  ( 0.000000000000000000, 0.1361666490962468723, -0.9906859460363306447 ) ) ;
#4597 = VERTEX_POINT ( 'NONE', #4015 ) ;
#4598 = CARTESIAN_POINT ( 'NONE',  ( 8.900000000000041211, 10.82531754730546147, 46.00000000000000711 ) ) ;
#4599 = CARTESIAN_POINT ( 'NONE',  ( 1.155036213957052500E-14, 4.618802153517020059, -5.599999999999999645 ) ) ;
#4600 = ORIENTED_EDGE ( 'NONE', *, *, #2739, .T. ) ;
#4601 = DIRECTION ( 'NONE',  ( 0.000000000000000000, -0.9976687691905384847, -0.06824241336468166164 ) ) ;
#4602 = CARTESIAN_POINT ( 'NONE',  ( 30.00000000000000000, -42.57363661491096707, 121.3828884801879155 ) ) ;
#4603 = VECTOR ( 'NONE', #6368, 1000.000000000000000 ) ;
#4604 = EDGE_LOOP ( 'NONE', ( #7890, #11418, #6378, #6773, #8023 ) ) ;
#4605 = CARTESIAN_POINT ( 'NONE',  ( 12.72792206288790950, 12.72792205982780089, -15.56957499981969129 ) ) ;
#4606 = DIRECTION ( 'NONE',  ( -1.000000000000000000, -0.000000000000000000, -0.000000000000000000 ) ) ;
#4607 = DIRECTION ( 'NONE',  ( 1.000000000000000000, -0.000000000000000000, -0.000000000000000000 ) ) ;
#4608 = ORIENTED_EDGE ( 'NONE', *, *, #2597, .T. ) ;
#4609 = DIRECTION ( 'NONE',  ( -0.000000000000000000, -0.000000000000000000, -1.000000000000000000 ) ) ;
#4610 = VERTEX_POINT ( 'NONE', #10496 ) ;
#4611 = CYLINDRICAL_SURFACE ( 'NONE', #15287, 72.00000000007199219 ) ;
#4612 = ORIENTED_EDGE ( 'NONE', *, *, #9538, .T. ) ;
#4613 = VECTOR ( 'NONE', #1190, 1000.000000000000000 ) ;
#4614 = DIRECTION ( 'NONE',  ( -0.000000000000000000, -0.000000000000000000, 1.000000000000000000 ) ) ;
#4615 = VECTOR ( 'NONE', #13420, 1000.000000000000000 ) ;
#4616 = VECTOR ( 'NONE', #16076, 1000.000000000000114 ) ;
#4617 = EDGE_CURVE ( 'NONE', #20554, #14177, #3749, .T. ) ;
#4618 = DIRECTION ( 'NONE',  ( 0.000000000000000000, 0.000000000000000000, 1.000000000000000000 ) ) ;
#4619 = CARTESIAN_POINT ( 'NONE',  ( -14.79893867758297610, 1.779018419858781159E-09, -17.24720808115845827 ) ) ;
#4620 = ORIENTED_EDGE ( 'NONE', *, *, #10209, .F. ) ;
#4621 = CARTESIAN_POINT ( 'NONE',  ( 6.358192987158592047, -4.248408730893246776, -17.59260624981969912 ) ) ;
#4622 = CIRCLE ( 'NONE', #18511, 7.500000000000000000 ) ;
#4623 = ORIENTED_EDGE ( 'NONE', *, *, #4820, .F. ) ;
#4624 = CARTESIAN_POINT ( 'NONE',  ( 21.03310778584661023, -4.548819502657031499, 88.88415356777898069 ) ) ;
#4625 = AXIS2_PLACEMENT_3D ( 'NONE', #19494, #3685, #13353 ) ;
#4626 = AXIS2_PLACEMENT_3D ( 'NONE', #7815, #14086, #20538 ) ;
#4627 = DIRECTION ( 'NONE',  ( 1.000000000000000000, 1.836909530733573776E-16, 0.000000000000000000 ) ) ;
#4628 = CARTESIAN_POINT ( 'NONE',  ( 2.500000000000000000, 0.000000000000000000, 0.000000000000000000 ) ) ;
#4629 = AXIS2_PLACEMENT_3D ( 'NONE', #15130, #20096, #3879 ) ;
#4630 = AXIS2_PLACEMENT_3D ( 'NONE', #16905, #16688, #2381 ) ;
#4631 = ORIENTED_EDGE ( 'NONE', *, *, #8540, .F. ) ;
#4632 =( GEOMETRIC_REPRESENTATION_CONTEXT ( 3 ) GLOBAL_UNCERTAINTY_ASSIGNED_CONTEXT ( ( #12390 ) ) GLOBAL_UNIT_ASSIGNED_CONTEXT ( ( #1927, #3811, #10297 ) ) REPRESENTATION_CONTEXT ( 'NONE', 'WORKASPACE' ) );
#4633 = CARTESIAN_POINT ( 'NONE',  ( -4.000000000000000000, 1.935983797701054998, -0.2494693066162268769 ) ) ;
#4634 = DIRECTION ( 'NONE',  ( 1.000000000000000000, 0.000000000000000000, -0.000000000000000000 ) ) ;
#4635 = ORIENTED_EDGE ( 'NONE', *, *, #5169, .F. ) ;
#4636 = CARTESIAN_POINT ( 'NONE',  ( -21.68676924570646847, -7.739453413396359061, -85.48199181195725771 ) ) ;
#4637 = CARTESIAN_POINT ( 'NONE',  ( -7.500000000000009770, 9.706494107251932559E-15, -16.92379999999768359 ) ) ;
#4638 = CARTESIAN_POINT ( 'NONE',  ( 17.99999999999999645, -2.163824016901520184E-09, -25.72104999981969442 ) ) ;
#4639 = ORIENTED_EDGE ( 'NONE', *, *, #5061, .T. ) ;
#4640 = CARTESIAN_POINT ( 'NONE',  ( 19.99999999999999645, -62.46228066917775834, -18.86519267363519958 ) ) ;
#4641 = DIRECTION ( 'NONE',  ( -1.000000000000000000, 0.000000000000000000, 0.000000000000000000 ) ) ;
#4642 = EDGE_CURVE ( 'NONE', #2640, #3596, #7141, .T. ) ;
#4643 = AXIS2_PLACEMENT_3D ( 'NONE', #14810, #5044, #9623 ) ;
#4644 = DIRECTION ( 'NONE',  ( -1.000000000000000000, 0.000000000000000000, 0.000000000000000000 ) ) ;
#4645 = DIRECTION ( 'NONE',  ( 0.7935941825507226710, -0.6084474286424838008, 1.243481486083095525E-31 ) ) ;
#4646 =( BOUNDED_CURVE ( )  B_SPLINE_CURVE ( 2, ( #6217, #17150, #10993, #12488, #18951, #17470, #4091, #18743, #10577, #2946, #17040, #20534, #19054, #6111, #8985, #942, #4421 ),
 .UNSPECIFIED., .F., .T. ) 
 B_SPLINE_CURVE_WITH_KNOTS ( ( 3, 2, 2, 2, 2, 2, 2, 2, 3 ),
 ( 0.3000000000038511860, 0.3125000000038511971, 0.3250000000038512082, 0.3375000000038512193, 0.3500000000038511749, 0.3625000000038511860, 0.3750000000038511971, 0.3875000000038512082, 0.4000000000038512193 ),
 .UNSPECIFIED. ) 
 CURVE ( )  GEOMETRIC_REPRESENTATION_ITEM ( )  RATIONAL_B_SPLINE_CURVE ( ( 0.9999999999940800688, 0.9807852804091503618, 1.000000000000000000, 0.9807852804032304306, 1.000000000000000000, 0.9807852804032304306, 1.000000000000000000, 0.9807852804032304306, 1.000000000000000000, 0.9807852804032304306, 1.000000000000000000, 0.9807852804032304306, 1.000000000000000000, 0.9807852804032304306, 1.000000000000000000, 0.9807852803973104994, 1.000000000005919931 ) ) 
 REPRESENTATION_ITEM ( '' )  );
#4647 = CARTESIAN_POINT ( 'NONE',  ( 16.62983158603122646, 6.888301780572504640, -5.555512499819690753 ) ) ;
#4648 = CIRCLE ( 'NONE', #11087, 2.041999999999999815 ) ;
#4649 = AXIS2_PLACEMENT_3D ( 'NONE', #3694, #15049, #3903 ) ;
#4650 = CARTESIAN_POINT ( 'NONE',  ( 5.303300858261588147, -5.303300859536636658, -20.45817499981968624 ) ) ;
#4651 = ORIENTED_EDGE ( 'NONE', *, *, #2610, .F. ) ;
#4652 = EDGE_CURVE ( 'NONE', #5613, #8436, #14606, .T. ) ;
#4653 = DIRECTION ( 'NONE',  ( -1.000000000000000000, 0.000000000000000000, 0.000000000000000000 ) ) ;
#4654 = EDGE_CURVE ( 'NONE', #16659, #540, #12299, .T. ) ;
#4655 = CARTESIAN_POINT ( 'NONE',  ( 9.474249097082495297, -6.330490858644137298, -27.44651600028680960 ) ) ;
#4656 = LINE ( 'NONE', #20858, #9490 ) ;
#4657 = APPLICATION_CONTEXT ( 'automotive_design' ) ;
#4658 = VECTOR ( 'NONE', #20125, 1000.000000000000000 ) ;
#4659 = VERTEX_POINT ( 'NONE', #9437 ) ;
#4660 = DIRECTION ( 'NONE',  ( 1.000000000000000000, 0.000000000000000000, 0.000000000000000000 ) ) ;
#4661 = AXIS2_PLACEMENT_3D ( 'NONE', #7228, #10320, #18067 ) ;
#4662 = CARTESIAN_POINT ( 'NONE',  ( 12.72792205982779734, -12.72792206288791128, -13.21332499981968667 ) ) ;
#4663 = CARTESIAN_POINT ( 'NONE',  ( 29.99999999999999289, -49.01438689058709741, 66.75225413593169321 ) ) ;
#4664 = ORIENTED_EDGE ( 'NONE', *, *, #19260, .T. ) ;
#4665 = DIRECTION ( 'NONE',  ( 0.000000000000000000, 0.000000000000000000, 1.000000000000000000 ) ) ;
#4666 = AXIS2_PLACEMENT_3D ( 'NONE', #9635, #6126, #17589 ) ;
#4667 = ORIENTED_EDGE ( 'NONE', *, *, #14660, .T. ) ;
#4668 = CARTESIAN_POINT ( 'NONE',  ( -24.99999999999999289, -85.00000000000000000, -1.040949779275250179E-14 ) ) ;
#4669 = FACE_OUTER_BOUND ( 'NONE', #14897, .T. ) ;
#4670 = ORIENTED_EDGE ( 'NONE', *, *, #10683, .T. ) ;
#4671 = VERTEX_POINT ( 'NONE', #1294 ) ;
#4672 = CARTESIAN_POINT ( 'NONE',  ( 32.33881229855617789, -114.4241705253154606, -75.39503781669127136 ) ) ;
#4673 = LINE ( 'NONE', #14217, #4165 ) ;
#4674 = AXIS2_PLACEMENT_3D ( 'NONE', #2790, #4162, #17102 ) ;
#4675 = CARTESIAN_POINT ( 'NONE',  ( 19.99999999999999645, -44.69367065308684062, 56.44887778834731051 ) ) ;
#4676 = CARTESIAN_POINT ( 'NONE',  ( -11.17563879704982988, 2.222972771497744748, -16.20035899935257362 ) ) ;
#4677 = EDGE_CURVE ( 'NONE', #9768, #2130, #18319, .T. ) ;
#4678 = CARTESIAN_POINT ( 'NONE',  ( 4.276731815070940357, 10.32494394706615815, 17.02770274971319964 ) ) ;
#4679 = EDGE_CURVE ( 'NONE', #16876, #9376, #1410, .T. ) ;
#4680 = CARTESIAN_POINT ( 'NONE',  ( 30.00000000000000000, -42.57363661491096707, -121.3828884801879155 ) ) ;
#4681 = DIRECTION ( 'NONE',  ( 1.000000000000000000, 0.000000000000000000, 0.000000000000000000 ) ) ;
#4682 = DIRECTION ( 'NONE',  ( -1.000000000000000000, 0.000000000000000000, 0.000000000000000000 ) ) ;
#4683 = EDGE_LOOP ( 'NONE', ( #12243, #5784, #12054, #1848 ) ) ;
#4684 = CARTESIAN_POINT ( 'NONE',  ( 0.000000000000000000, 0.000000000000000000, 166.0000000000000000 ) ) ;
#4685 = VERTEX_POINT ( 'NONE', #6139 ) ;
#4686 = CARTESIAN_POINT ( 'NONE',  ( -15.25966316918061771, 10.19618095414378622, -20.12495624981968945 ) ) ;
#4687 = DIRECTION ( 'NONE',  ( 0.000000000000000000, 0.000000000000000000, -1.000000000000000000 ) ) ;
#4688 = EDGE_CURVE ( 'NONE', #12530, #16309, #17654, .T. ) ;
#4689 = ORIENTED_EDGE ( 'NONE', *, *, #9726, .T. ) ;
#4690 = LINE ( 'NONE', #11150, #15701 ) ;
#4691 = ORIENTED_EDGE ( 'NONE', *, *, #14542, .F. ) ;
#4692 = CARTESIAN_POINT ( 'NONE',  ( 0.2500000000000002220, 0.000000000000000000, 0.000000000000000000 ) ) ;
#4693 = DIRECTION ( 'NONE',  ( 0.000000000000000000, 0.000000000000000000, -1.000000000000000000 ) ) ;
#4694 = DIRECTION ( 'NONE',  ( 0.000000000000000000, 0.9422609221188213979, -0.3348796121709835538 ) ) ;
#4695 = ORIENTED_EDGE ( 'NONE', *, *, #14857, .F. ) ;
#4696 = FACE_OUTER_BOUND ( 'NONE', #5503, .T. ) ;
#4697 = DIRECTION ( 'NONE',  ( -1.000000000000000000, 0.000000000000000000, 0.000000000000000000 ) ) ;
#4698 = FACE_OUTER_BOUND ( 'NONE', #1672, .T. ) ;
#4699 = EDGE_CURVE ( 'NONE', #5439, #14211, #8485, .T. ) ;
#4700 = DIRECTION ( 'NONE',  ( -1.000000000000000000, 1.734723475976807094E-16, 0.000000000000000000 ) ) ;
#4701 = ORIENTED_EDGE ( 'NONE', *, *, #10454, .F. ) ;
#4702 = EDGE_CURVE ( 'NONE', #15842, #2254, #4084, .T. ) ;
#4703 = DIRECTION ( 'NONE',  ( -1.000000000000000000, 0.000000000000000000, 0.000000000000000000 ) ) ;
#4704 = EDGE_CURVE ( 'NONE', #8657, #18161, #3412, .T. ) ;
#4705 = CARTESIAN_POINT ( 'NONE',  ( -5.303300859536636658, -5.303300858261589035, 0.7480750001803149196 ) ) ;
#4706 = VERTEX_POINT ( 'NONE', #7516 ) ;
#4707 = DIRECTION ( 'NONE',  ( 0.000000000000000000, 0.000000000000000000, -1.000000000000000000 ) ) ;
#4708 = CARTESIAN_POINT ( 'NONE',  ( 3.599999999999909051, -10.82531754730554496, 46.00000000000000711 ) ) ;
#4709 = EDGE_CURVE ( 'NONE', #5222, #2180, #6791, .T. ) ;
#4710 = VERTEX_POINT ( 'NONE', #20457 ) ;
#4711 = CARTESIAN_POINT ( 'NONE',  ( 0.000000000000000000, 0.000000000000000000, 90.00000000000000000 ) ) ;
#4712 = DIRECTION ( 'NONE',  ( -1.000000000000000000, -0.000000000000000000, -0.000000000000000000 ) ) ;
#4713 = CARTESIAN_POINT ( 'NONE',  ( 0.6543461111163461075, 4.241015250120812929, -0.1391502195351438376 ) ) ;
#4714 = EDGE_LOOP ( 'NONE', ( #14546, #16819, #2635, #17037 ) ) ;
#4715 = DIRECTION ( 'NONE',  ( 0.000000000000000000, 0.000000000000000000, 1.000000000000000000 ) ) ;
#4716 = ORIENTED_EDGE ( 'NONE', *, *, #388, .F. ) ;
#4717 = CARTESIAN_POINT ( 'NONE',  ( -31.75000000000000000, -10.52399999999999380, 1.288818291422673781E-15 ) ) ;
#4718 = ORIENTED_EDGE ( 'NONE', *, *, #5202, .T. ) ;
#4719 = DIRECTION ( 'NONE',  ( 0.000000000000000000, 0.000000000000000000, 1.000000000000000000 ) ) ;
#4720 = EDGE_CURVE ( 'NONE', #19863, #18058, #20338, .T. ) ;
#4721 = CARTESIAN_POINT ( 'NONE',  ( 0.000000000000000000, 58.44960523466241398, 28.06621538408611016 ) ) ;
#4722 = CARTESIAN_POINT ( 'NONE',  ( 12.54593441562640876, -8.382925371439629458, -11.65111433115845863 ) ) ;
#4723 = VERTEX_POINT ( 'NONE', #15893 ) ;
#4724 = CARTESIAN_POINT ( 'NONE',  ( 40.00000000000000711, -40.00000000000001421, -120.0000000000000142 ) ) ;
#4725 = EDGE_CURVE ( 'NONE', #6520, #5761, #6124, .T. ) ;
#4726 = DIRECTION ( 'NONE',  ( 0.000000000000000000, 0.000000000000000000, 1.000000000000000000 ) ) ;
#4727 = VERTEX_POINT ( 'NONE', #20761 ) ;
#4728 = CARTESIAN_POINT ( 'NONE',  ( 19.08980715481771995, -9.906743869288808568, 83.52356801772648964 ) ) ;
#4729 = CARTESIAN_POINT ( 'NONE',  ( -3.580422610670018546, 18.00000000043041126, 20.65776875018031333 ) ) ;
#4730 = DIRECTION ( 'NONE',  ( 0.000000000000000000, 0.000000000000000000, 1.000000000000000000 ) ) ;
#4731 = DIRECTION ( 'NONE',  ( -1.000000000000000000, -0.000000000000000000, -0.000000000000000000 ) ) ;
#4732 = CIRCLE ( 'NONE', #16246, 14.49999999999999822 ) ;
#4733 = EDGE_LOOP ( 'NONE', ( #15951, #17348, #5692, #9180 ) ) ;
#4734 = EDGE_CURVE ( 'NONE', #8346, #8326, #11537, .T. ) ;
#4735 = CARTESIAN_POINT ( 'NONE',  ( -30.00000000000000000, -105.0000000000000284, -77.45966692414833688 ) ) ;
#4736 = DIRECTION ( 'NONE',  ( 1.000000000000000000, 0.000000000000000000, 0.000000000000000000 ) ) ;
#4737 = EDGE_LOOP ( 'NONE', ( #8988, #2837, #18735, #12960 ) ) ;
#4738 = CARTESIAN_POINT ( 'NONE',  ( 0.000000000000000000, 0.000000000000000000, -130.0000000000000000 ) ) ;
#4739 = CARTESIAN_POINT ( 'NONE',  ( 19.99999999999999645, 0.000000000000000000, 0.000000000000000000 ) ) ;
#4740 = CARTESIAN_POINT ( 'NONE',  ( -3.580422614997674557, -17.99999999956957808, -23.07026874981968945 ) ) ;
#4741 = ORIENTED_EDGE ( 'NONE', *, *, #3767, .T. ) ;
#4742 = DIRECTION ( 'NONE',  ( 1.202124453834178339E-10, 1.000000000000000000, -4.318160619762183323E-26 ) ) ;
#4743 = CARTESIAN_POINT ( 'NONE',  ( 19.99999999999999645, 0.000000000000000000, 0.000000000000000000 ) ) ;
#4744 = DIRECTION ( 'NONE',  ( -1.000000000000000000, 0.000000000000000000, -6.982962677686266711E-15 ) ) ;
#4745 = CARTESIAN_POINT ( 'NONE',  ( 15.25966316918061771, -10.19618095414378800, -4.082856249819691641 ) ) ;
#4746 = CARTESIAN_POINT ( 'NONE',  ( 19.99999999999999645, -5.762283366691622000, 64.99406197038668154 ) ) ;
#4747 = CARTESIAN_POINT ( 'NONE',  ( 50.00000000000000000, -139.6410161513775563, -90.00000000000001421 ) ) ;
#4748 = CARTESIAN_POINT ( 'NONE',  ( 8.382925368423265411, -12.54593441764187034, -7.255135668480925837 ) ) ;
#4749 = CARTESIAN_POINT ( 'NONE',  ( -65.00002539999999840, 0.000000000000000000, 0.000000000000000000 ) ) ;
#4750 = AXIS2_PLACEMENT_3D ( 'NONE', #2245, #654, #7103 ) ;
#4751 = EDGE_CURVE ( 'NONE', #20537, #20612, #12359, .T. ) ;
#4752 = ORIENTED_EDGE ( 'NONE', *, *, #18112, .F. ) ;
#4753 = EDGE_CURVE ( 'NONE', #4894, #3991, #1086, .T. ) ;
#4754 = CARTESIAN_POINT ( 'NONE',  ( 19.99999999999999645, 39.37110852956887186, -51.51683813304829584 ) ) ;
#4755 = CARTESIAN_POINT ( 'NONE',  ( 6.249999999999902300, -10.82531754730554496, -43.00000000000000000 ) ) ;
#4756 = CARTESIAN_POINT ( 'NONE',  ( 31.45428956093201123, -36.32466546818508135, 66.70503744075557506 ) ) ;
#4757 = VERTEX_POINT ( 'NONE', #16305 ) ;
#4758 = DIRECTION ( 'NONE',  ( 0.000000000000000000, -0.1361666490962539222, 0.9906859460363298675 ) ) ;
#4759 = ORIENTED_EDGE ( 'NONE', *, *, #5809, .F. ) ;
#4760 = LINE ( 'NONE', #16110, #62 ) ;
#4761 = CARTESIAN_POINT ( 'NONE',  ( 19.99999999999999645, 63.85430960833490843, -11.25592921604860663 ) ) ;
#4762 = VECTOR ( 'NONE', #9030, 1000.000000000000000 ) ;
#4763 = EDGE_LOOP ( 'NONE', ( #18938, #7814, #10914, #12327 ) ) ;
#4764 = EDGE_LOOP ( 'NONE', ( #6815, #12237, #2023, #13533 ) ) ;
#4765 = CARTESIAN_POINT ( 'NONE',  ( 47.39552796998189166, -5.594374250344187338, 80.66125912922146313 ) ) ;
#4766 = VECTOR ( 'NONE', #2246, 1000.000000000000000 ) ;
#4767 = AXIS2_PLACEMENT_3D ( 'NONE', #11893, #3832, #13819 ) ;
#4768 = CARTESIAN_POINT ( 'NONE',  ( 3.600000000000060485, 10.82531754730546147, 46.00000000000000711 ) ) ;
#4769 = CARTESIAN_POINT ( 'NONE',  ( 4.000000000000004441, -1.549102112939112486, -0.1578953385959447620 ) ) ;
#4770 = CARTESIAN_POINT ( 'NONE',  ( -9.474249098604513364, -6.330490856366295382, -17.37848399935257859 ) ) ;
#4771 = ADVANCED_FACE ( 'NONE', ( #11444 ), #19278, .T. ) ;
#4772 = CARTESIAN_POINT ( 'NONE',  ( -10.32494394809439164, -4.276731812588563386, 4.068327749713199104 ) ) ;
#4773 = CARTESIAN_POINT ( 'NONE',  ( 0.000000000000000000, -35.35772184876915958, 54.34979580218180928 ) ) ;
#4774 = CARTESIAN_POINT ( 'NONE',  ( 0.000000000000000000, 0.000000000000000000, 0.000000000000000000 ) ) ;
#4775 = DIRECTION ( 'NONE',  ( -1.000000000000000000, -0.000000000000000000, 0.000000000000000000 ) ) ;
#4776 = AXIS2_PLACEMENT_3D ( 'NONE', #14795, #17880, #17775 ) ;
#4777 = ORIENTED_EDGE ( 'NONE', *, *, #13561, .T. ) ;
#4778 = DIRECTION ( 'NONE',  ( -1.000000000000000000, 0.000000000000000000, 0.000000000000000000 ) ) ;
#4779 = VERTEX_POINT ( 'NONE', #3280 ) ;
#4780 = CARTESIAN_POINT ( 'NONE',  ( 12.72792206288790950, 12.72792205982780089, 22.13042500018031689 ) ) ;
#4781 = CARTESIAN_POINT ( 'NONE',  ( 49.35000000000000142, -99.99999999999998579, 5.000000000000000000 ) ) ;
#4782 = AXIS2_PLACEMENT_3D ( 'NONE', #2974, #5936, #17283 ) ;
#4783 = VERTEX_POINT ( 'NONE', #1501 ) ;
#4784 = DIRECTION ( 'NONE',  ( -1.000000000000000000, 0.000000000000000000, 0.000000000000000000 ) ) ;
#4785 = ORIENTED_EDGE ( 'NONE', *, *, #16066, .T. ) ;
#4786 = CARTESIAN_POINT ( 'NONE',  ( 19.99999999999999645, 64.80702306891106446, -7.581672767545749814 ) ) ;
#4787 = CARTESIAN_POINT ( 'NONE',  ( 0.000000000000000000, -49.77519642623978058, -42.18840861821836796 ) ) ;
#4788 = ORIENTED_EDGE ( 'NONE', *, *, #4292, .T. ) ;
#4789 = ORIENTED_EDGE ( 'NONE', *, *, #10454, .T. ) ;
#4790 = DIRECTION ( 'NONE',  ( 1.000000000000000000, 1.836909530733573776E-16, 0.000000000000000000 ) ) ;
#4791 = EDGE_CURVE ( 'NONE', #6575, #9434, #16308, .T. ) ;
#4792 = EDGE_CURVE ( 'NONE', #7461, #1037, #4760, .T. ) ;
#4793 = DIRECTION ( 'NONE',  ( -0.5000000000000037748, -0.8660254037844364872, 0.000000000000000000 ) ) ;
#4794 = CARTESIAN_POINT ( 'NONE',  ( 4.000000000000004441, 0.7862748000878159171, -0.03447227762756879116 ) ) ;
#4795 = CIRCLE ( 'NONE', #11601, 49.99999999999998579 ) ;
#4796 = VECTOR ( 'NONE', #11789, 1000.000000000000000 ) ;
#4797 = CARTESIAN_POINT ( 'NONE',  ( -12.50000000000000533, 0.000000000000000000, 46.00000000000000711 ) ) ;
#4798 = CIRCLE ( 'NONE', #19349, 65.24900000006525147 ) ;
#4799 = ADVANCED_FACE ( 'NONE', ( #11229 ), #3372, .T. ) ;
#4800 = ORIENTED_EDGE ( 'NONE', *, *, #2365, .T. ) ;
#4801 = DIRECTION ( 'NONE',  ( -1.000000000000000000, -0.000000000000000000, -0.000000000000000000 ) ) ;
#4802 = CARTESIAN_POINT ( 'NONE',  ( -2.870125743571144028, -6.929096493489630859, 0.1590125001803138760 ) ) ;
#4803 = CIRCLE ( 'NONE', #17339, 27.60000000002760245 ) ;
#4804 = CARTESIAN_POINT ( 'NONE',  ( 50.00000000000000000, 4.299168419249259188, -90.00000000000000000 ) ) ;
#4805 = DIRECTION ( 'NONE',  ( 0.000000000000000000, 0.000000000000000000, 1.000000000000000000 ) ) ;
#4806 = ORIENTED_EDGE ( 'NONE', *, *, #5276, .T. ) ;
#4807 = DIRECTION ( 'NONE',  ( 0.000000000000000000, 0.000000000000000000, 1.000000000000000000 ) ) ;
#4808 = CARTESIAN_POINT ( 'NONE',  ( 0.000000000000000000, 0.000000000000000000, 0.000000000000000000 ) ) ;
#4809 = LINE ( 'NONE', #11277, #20091 ) ;
#4810 = CIRCLE ( 'NONE', #2767, 2.649999999999999467 ) ;
#4811 = EDGE_LOOP ( 'NONE', ( #7573, #362, #19048, #4329 ) ) ;
#4812 = VECTOR ( 'NONE', #14227, 1000.000000000000000 ) ;
#4813 = FACE_BOUND ( 'NONE', #3094, .T. ) ;
#4814 = ORIENTED_EDGE ( 'NONE', *, *, #15573, .F. ) ;
#4815 = LINE ( 'NONE', #17559, #15975 ) ;
#4816 = EDGE_LOOP ( 'NONE', ( #13117, #15122, #2483, #11721 ) ) ;
#4817 = EDGE_CURVE ( 'NONE', #7659, #9981, #9874, .T. ) ;
#4818 = EDGE_CURVE ( 'NONE', #10364, #4779, #2417, .T. ) ;
#4819 = DIRECTION ( 'NONE',  ( -0.000000000000000000, -0.000000000000000000, -1.000000000000000000 ) ) ;
#4820 = EDGE_CURVE ( 'NONE', #7472, #12251, #6354, .T. ) ;
#4821 = LINE ( 'NONE', #11290, #8222 ) ;
#4822 = CARTESIAN_POINT ( 'NONE',  ( -4.276731812588566939, 10.32494394809439875, 22.97229725064743278 ) ) ;
#4823 = AXIS2_PLACEMENT_3D ( 'NONE', #9309, #1479, #19063 ) ;
#4825 = ORIENTED_EDGE ( 'NONE', *, *, #12340, .T. ) ;
#4824 = AXIS2_PLACEMENT_3D ( 'NONE', #5602, #10711, #12082 ) ;
#4826 = PLANE ( 'NONE',  #6584 ) ;
#4827 = AXIS2_PLACEMENT_3D ( 'NONE', #6744, #3166, #10047 ) ;
#4828 = FACE_BOUND ( 'NONE', #17724, .T. ) ;
#4829 = VECTOR ( 'NONE', #5253, 1000.000000000000000 ) ;
#4830 = ORIENTED_EDGE ( 'NONE', *, *, #14562, .F. ) ;
#4831 = CARTESIAN_POINT ( 'NONE',  ( 11.69263306866421814, -18.04574728598160505, 77.81190555643075868 ) ) ;
#4832 = DIRECTION ( 'NONE',  ( -1.000000000000000000, -0.000000000000000000, -0.000000000000000000 ) ) ;
#4833 = FACE_OUTER_BOUND ( 'NONE', #16559, .T. ) ;
#4834 = DIRECTION ( 'NONE',  ( 0.000000000000000000, 0.000000000000000000, 1.000000000000000000 ) ) ;
#4835 = EDGE_CURVE ( 'NONE', #9196, #5499, #9533, .T. ) ;
#4836 = ADVANCED_FACE ( 'NONE', ( #304 ), #19686, .T. ) ;
#4837 = ORIENTED_EDGE ( 'NONE', *, *, #12432, .F. ) ;
#4838 = FACE_OUTER_BOUND ( 'NONE', #368, .T. ) ;
#4839 = EDGE_LOOP ( 'NONE', ( #8170, #6992, #11580, #5017 ) ) ;
#4840 = VECTOR ( 'NONE', #3755, 1000.000000000000000 ) ;
#4841 = DIRECTION ( 'NONE',  ( -0.000000000000000000, -0.000000000000000000, 1.000000000000000000 ) ) ;
#4842 = AXIS2_PLACEMENT_3D ( 'NONE', #12724, #19177, #17594 ) ;
#4843 = CYLINDRICAL_SURFACE ( 'NONE', #11026, 200.0000000000000000 ) ;
#4844 = CARTESIAN_POINT ( 'NONE',  ( 7.500000000000009770, 1.491842754878799138, -3.080831249912204584 ) ) ;
#4845 = ADVANCED_FACE ( 'NONE', ( #9649, #18110, #11340, #13143, #7950, #8057 ), #3577, .F. ) ;
#4846 = ORIENTED_EDGE ( 'NONE', *, *, #5155, .T. ) ;
#4847 = DIRECTION ( 'NONE',  ( 1.000000000000000000, 0.000000000000000000, 0.000000000000000000 ) ) ;
#4848 = PRESENTATION_STYLE_ASSIGNMENT (( #11803 ) ) ;
#4849 = LINE ( 'NONE', #17369, #20386 ) ;
#4850 = CARTESIAN_POINT ( 'NONE',  ( -12.50000000000000711, 1.734723475976807094E-13, -51.00000000000001421 ) ) ;
#4851 = AXIS2_PLACEMENT_3D ( 'NONE', #4761, #9943, #6660 ) ;
#4852 = CARTESIAN_POINT ( 'NONE',  ( 3.580422610670021211, -18.00000000043041481, -12.32973124981968915 ) ) ;
#4853 = VECTOR ( 'NONE', #5721, 1000.000000000000000 ) ;
#4854 = ORIENTED_EDGE ( 'NONE', *, *, #1986, .F. ) ;
#4855 = FACE_OUTER_BOUND ( 'NONE', #19680, .T. ) ;
#4856 = AXIS2_PLACEMENT_3D ( 'NONE', #15196, #13828, #5649 ) ;
#4857 = DIRECTION ( 'NONE',  ( 1.000000000000000000, 1.836909530733573776E-16, 0.000000000000000000 ) ) ;
#4858 = VECTOR ( 'NONE', #12114, 1000.000000000000000 ) ;
#4859 = CARTESIAN_POINT ( 'NONE',  ( -10.46442989202483709, 10.46442989454075168, -12.26216691848092744 ) ) ;
#4860 = ORIENTED_EDGE ( 'NONE', *, *, #10122, .F. ) ;
#4861 = DIRECTION ( 'NONE',  ( 0.000000000000000000, 0.000000000000000000, -1.000000000000000000 ) ) ;
#4862 = CARTESIAN_POINT ( 'NONE',  ( 7.500000000000000000, -9.015933403756343749E-10, 25.48870000018031590 ) ) ;
#4863 = CARTESIAN_POINT ( 'NONE',  ( 2.500000000000002220, 3.061616997868386099E-16, -5.574599999999999334 ) ) ;
#4864 = CIRCLE ( 'NONE', #9275, 17.50000000000000355 ) ;
#4865 = ORIENTED_EDGE ( 'NONE', *, *, #8954, .T. ) ;
#4866 = CIRCLE ( 'NONE', #16039, 23.00000000000000000 ) ;
#4867 = FACE_OUTER_BOUND ( 'NONE', #4737, .T. ) ;
#4868 = AXIS2_PLACEMENT_3D ( 'NONE', #2695, #12668, #16048 ) ;
#4869 = ORIENTED_EDGE ( 'NONE', *, *, #14144, .T. ) ;
#4870 = DIRECTION ( 'NONE',  ( -1.000000000000000000, 0.000000000000000000, 0.000000000000000000 ) ) ;
#4871 = CARTESIAN_POINT ( 'NONE',  ( -15.25966316918061416, 10.19618095414378445, 17.57504375018031340 ) ) ;
#4872 = ORIENTED_EDGE ( 'NONE', *, *, #8954, .F. ) ;
#4873 = ORIENTED_EDGE ( 'NONE', *, *, #572, .F. ) ;
#4874 = DIRECTION ( 'NONE',  ( -1.000000000000000000, -0.000000000000000000, -0.000000000000000000 ) ) ;
#4875 = CIRCLE ( 'NONE', #131, 17.50000000000000355 ) ;
#4876 = CIRCLE ( 'NONE', #2502, 4.250000000000000000 ) ;
#4877 = AXIS2_PLACEMENT_3D ( 'NONE', #143, #16356, #17860 ) ;
#4878 = CARTESIAN_POINT ( 'NONE',  ( 0.000000000000000000, -1.971042061628798470, 64.80882494896106039 ) ) ;
#4879 = CARTESIAN_POINT ( 'NONE',  ( 0.2500000000000002220, 0.000000000000000000, 4.000000000000000000 ) ) ;
#4880 = EDGE_CURVE ( 'NONE', #13026, #11744, #12932, .T. ) ;
#4881 = CARTESIAN_POINT ( 'NONE',  ( 50.00000000000000000, -110.0000000000000142, 44.99999999999999289 ) ) ;
#4882 = CARTESIAN_POINT ( 'NONE',  ( -5.303300859536636658, -5.303300858261589035, 19.59807500018031590 ) ) ;
#4883 = VECTOR ( 'NONE', #17104, 1000.000000000000000 ) ;
#4884 = CARTESIAN_POINT ( 'NONE',  ( -2.222972768810836275, 11.17563879758427525, 6.719108999713199637 ) ) ;
#4885 = CARTESIAN_POINT ( 'NONE',  ( 19.99999999999999645, 64.52323195238628273, 6.389157729493382121 ) ) ;
#4886 = CIRCLE ( 'NONE', #16725, 2.500000000000002220 ) ;
#4887 = DIRECTION ( 'NONE',  ( -0.000000000000000000, -0.000000000000000000, 1.000000000000000000 ) ) ;
#4888 = DIRECTION ( 'NONE',  ( -0.000000000000000000, -0.000000000000000000, -1.000000000000000000 ) ) ;
#4889 = VECTOR ( 'NONE', #18790, 1000.000000000000000 ) ;
#4890 = ORIENTED_EDGE ( 'NONE', *, *, #4404, .T. ) ;
#4891 = CARTESIAN_POINT ( 'NONE',  ( 19.99999999999999645, -56.63599015375694989, 31.56633360682443268 ) ) ;
#4892 = CARTESIAN_POINT ( 'NONE',  ( 12.72792206288790950, 12.72792205982780089, 12.70542500018031262 ) ) ;
#4893 = PLANE ( 'NONE',  #6570 ) ;
#4894 = VERTEX_POINT ( 'NONE', #8145 ) ;
#4895 = FACE_OUTER_BOUND ( 'NONE', #9617, .T. ) ;
#4896 = ORIENTED_EDGE ( 'NONE', *, *, #7082, .T. ) ;
#4897 = DIRECTION ( 'NONE',  ( -0.000000000000000000, -0.000000000000000000, 1.000000000000000000 ) ) ;
#4898 = CARTESIAN_POINT ( 'NONE',  ( 9.999999999999998224, -63.48283426024875808, 33.96954156735348107 ) ) ;
#4899 = ORIENTED_EDGE ( 'NONE', *, *, #16885, .T. ) ;
#4900 = ORIENTED_EDGE ( 'NONE', *, *, #2945, .T. ) ;
#4901 = DIRECTION ( 'NONE',  ( -0.000000000000000000, -0.000000000000000000, -1.000000000000000000 ) ) ;
#4902 = CARTESIAN_POINT ( 'NONE',  ( 19.99999999999999645, 67.51707036274413554, 25.00890260772400708 ) ) ;
#4903 = CIRCLE ( 'NONE', #17101, 27.60000000002759180 ) ;
#4904 = ADVANCED_FACE ( 'NONE', ( #95 ), #13034, .T. ) ;
#4905 = DIRECTION ( 'NONE',  ( 0.000000000000000000, 1.000000000000000000, -1.287488025362403787E-15 ) ) ;
#4906 = ORIENTED_EDGE ( 'NONE', *, *, #18663, .T. ) ;
#4907 = CARTESIAN_POINT ( 'NONE',  ( 7.500000000000000888, -9.015933403756337545E-10, 19.22380000018031154 ) ) ;
#4908 = DIRECTION ( 'NONE',  ( 1.836909530733573776E-16, -1.000000000000000000, 0.000000000000000000 ) ) ;
#4909 = AXIS2_PLACEMENT_3D ( 'NONE', #19165, #15773, #7612 ) ;
#4910 = DIRECTION ( 'NONE',  ( -1.000000000000000000, 0.000000000000000000, 0.000000000000000000 ) ) ;
#4911 = DIRECTION ( 'NONE',  ( 0.000000000000000000, -0.9422609221188237294, 0.3348796121709771700 ) ) ;
#4912 = EDGE_CURVE ( 'NONE', #10368, #12559, #11528, .T. ) ;
#4913 = ORIENTED_EDGE ( 'NONE', *, *, #7784, .F. ) ;
#4914 = DIRECTION ( 'NONE',  ( -0.000000000000000000, -0.000000000000000000, 1.000000000000000000 ) ) ;
#4915 = CARTESIAN_POINT ( 'NONE',  ( -15.25966317163203279, -10.19618095047498052, 15.80785625018031659 ) ) ;
#4916 = CARTESIAN_POINT ( 'NONE',  ( 19.99999999999999645, -51.81019761368347787, 38.98425606966041101 ) ) ;
#4917 = ORIENTED_EDGE ( 'NONE', *, *, #9430, .F. ) ;
#4918 = CARTESIAN_POINT ( 'NONE',  ( 0.000000000000000000, 0.000000000000000000, -0.2800830152838832965 ) ) ;
#4919 = ORIENTED_EDGE ( 'NONE', *, *, #6891, .F. ) ;
#4920 = AXIS2_PLACEMENT_3D ( 'NONE', #10436, #15300, #15199 ) ;
#4921 = DIRECTION ( 'NONE',  ( -1.000000000000000000, 0.000000000000000000, 0.000000000000000000 ) ) ;
#4922 = ORIENTED_EDGE ( 'NONE', *, *, #10129, .T. ) ;
#4923 = CARTESIAN_POINT ( 'NONE',  ( 39.24629858617094413, -121.8853583615259311, 79.93655681056323203 ) ) ;
#4924 = LINE ( 'NONE', #1751, #8905 ) ;
#4925 =( REPRESENTATION_RELATIONSHIP ('NONE','NONE', #13739, #9416 ) REPRESENTATION_RELATIONSHIP_WITH_TRANSFORMATION ( #13738 )SHAPE_REPRESENTATION_RELATIONSHIP( ) );
#4926 = CARTESIAN_POINT ( 'NONE',  ( -6.330490858644140850, -9.474249097082498849, 19.73245350064743420 ) ) ;
#4927 = ORIENTED_EDGE ( 'NONE', *, *, #2081, .F. ) ;
#4928 = DIRECTION ( 'NONE',  ( 1.000000000000000000, -0.000000000000000000, 0.000000000000000000 ) ) ;
#4929 = EDGE_CURVE ( 'NONE', #17883, #1644, #16636, .T. ) ;
#4930 = CARTESIAN_POINT ( 'NONE',  ( 6.232799999999996565, 0.000000000000000000, 0.000000000000000000 ) ) ;
#4931 = VERTEX_POINT ( 'NONE', #11747 ) ;
#4932 = CARTESIAN_POINT ( 'NONE',  ( 19.99999999999999645, -48.70996102988709708, 42.79495875147758710 ) ) ;
#4933 = EDGE_CURVE ( 'NONE', #20492, #16575, #10897, .T. ) ;
#4934 = EDGE_CURVE ( 'NONE', #19113, #2910, #18335, .T. ) ;
#4935 = CARTESIAN_POINT ( 'NONE',  ( 2.163825119083639534E-09, 18.00000000000000000, 20.95230000018031546 ) ) ;
#4936 = DIRECTION ( 'NONE',  ( 1.000000000000000000, 0.000000000000000000, 0.000000000000000000 ) ) ;
#4937 = CARTESIAN_POINT ( 'NONE',  ( -10.00000000000000000, 0.000000000000000000, 0.000000000000000000 ) ) ;
#4938 = VERTEX_POINT ( 'NONE', #3885 ) ;
#4939 = CIRCLE ( 'NONE', #1241, 7.500000000000000000 ) ;
#4940 = EDGE_CURVE ( 'NONE', #16324, #17864, #18668, .T. ) ;
#4941 = CARTESIAN_POINT ( 'NONE',  ( 85.00002539999999840, 0.000000000000000000, 0.000000000000000000 ) ) ;
#4942 = ADVANCED_FACE ( 'NONE', ( #19991 ), #16927, .T. ) ;
#4943 = ORIENTED_EDGE ( 'NONE', *, *, #13811, .T. ) ;
#4944 = CARTESIAN_POINT ( 'NONE',  ( 50.00100000000000477, -85.00000000000000000, -1.040949779275250179E-14 ) ) ;
#4945 = AXIS2_PLACEMENT_3D ( 'NONE', #5036, #8520, #19873 ) ;
#4946 = CIRCLE ( 'NONE', #7655, 2.649999999999994582 ) ;
#4947 = DIRECTION ( 'NONE',  ( 1.000000000000000000, 0.000000000000000000, 0.000000000000000000 ) ) ;
#4948 = CARTESIAN_POINT ( 'NONE',  ( 6.888301780572505528, -16.62983158603121581, -23.95386249981969229 ) ) ;
#4949 = ORIENTED_EDGE ( 'NONE', *, *, #6075, .T. ) ;
#4950 = DIRECTION ( 'NONE',  ( -0.000000000000000000, -0.000000000000000000, 1.000000000000000000 ) ) ;
#4951 = CIRCLE ( 'NONE', #8663, 27.60000000002760245 ) ;
#4952 = DIRECTION ( 'NONE',  ( 0.000000000000000000, 1.000000000000000000, 0.000000000000000000 ) ) ;
#4953 = CARTESIAN_POINT ( 'NONE',  ( -10.19618095414378800, -15.25966316918061771, -20.57660624981969733 ) ) ;
#4954 = ADVANCED_FACE ( 'NONE', ( #16609 ), #15343, .T. ) ;
#4955 = ORIENTED_EDGE ( 'NONE', *, *, #7126, .F. ) ;
#4956 = AXIS2_PLACEMENT_3D ( 'NONE', #10582, #521, #2532 ) ;
#4957 = DIRECTION ( 'NONE',  ( 0.000000000000000000, 0.3984010898462361228, 0.9172113015054554896 ) ) ;
#4958 = EDGE_CURVE ( 'NONE', #20612, #16461, #8764, .T. ) ;
#4959 = CIRCLE ( 'NONE', #7324, 10.79377999999999993 ) ;
#4960 = AXIS2_PLACEMENT_3D ( 'NONE', #14391, #19351, #20834 ) ;
#4961 = CARTESIAN_POINT ( 'NONE',  ( 5.663308650141530620, 13.67243654642775041, -10.49497941848093063 ) ) ;
#4962 = ADVANCED_FACE ( 'NONE', ( #2099 ), #10365, .F. ) ;
#4963 = CARTESIAN_POINT ( 'NONE',  ( 0.000000000000000000, 0.000000000000000000, -68.00000000000000000 ) ) ;
#4964 = EDGE_CURVE ( 'NONE', #18976, #14272, #3992, .T. ) ;
#4965 = ORIENTED_EDGE ( 'NONE', *, *, #1854, .T. ) ;
#4966 = DIRECTION ( 'NONE',  ( 1.000000000000000000, 0.000000000000000000, 0.000000000000000000 ) ) ;
#4967 = TOROIDAL_SURFACE ( 'NONE', #19522, 7.567219999999999835, 0.06721999999999891950 ) ;
#4968 = CARTESIAN_POINT ( 'NONE',  ( -4.248408729364580694, 6.358192988180020322, 22.24885625018031732 ) ) ;
#4969 = DIRECTION ( 'NONE',  ( -1.000000000000000000, 0.000000000000000000, 0.000000000000000000 ) ) ;
#4970 = ORIENTED_EDGE ( 'NONE', *, *, #14140, .F. ) ;
#4971 = DIRECTION ( 'NONE',  ( -1.000000000000000000, 0.000000000000000000, -0.000000000000000000 ) ) ;
#4972 = AXIS2_PLACEMENT_3D ( 'NONE', #19997, #18430, #8770 ) ;
#4973 = VERTEX_POINT ( 'NONE', #18423 ) ;
#4974 = CARTESIAN_POINT ( 'NONE',  ( 30.00000000000000000, -85.00000000000000000, -1.040949779275250179E-14 ) ) ;
#4975 = CARTESIAN_POINT ( 'NONE',  ( 24.99999999999999645, -39.99999999999999289, 54.09999999999999432 ) ) ;
#4976 = CIRCLE ( 'NONE', #591, 35.00000000000001421 ) ;
#4977 = ORIENTED_EDGE ( 'NONE', *, *, #6647, .T. ) ;
#4978 = ORIENTED_EDGE ( 'NONE', *, *, #17259, .T. ) ;
#4979 = CARTESIAN_POINT ( 'NONE',  ( 46.24771825328784303, -7.470032835629814016, -79.01456834021801967 ) ) ;
#4980 = VECTOR ( 'NONE', #18845, 1000.000000000000000 ) ;
#4981 = CIRCLE ( 'NONE', #8693, 2.649999999999992806 ) ;
#4982 = DIRECTION ( 'NONE',  ( -1.000000000000000000, 0.000000000000000000, 0.000000000000000000 ) ) ;
#4983 =( NAMED_UNIT ( * ) PLANE_ANGLE_UNIT ( ) SI_UNIT ( $, .RADIAN. ) );
#4984 = DIRECTION ( 'NONE',  ( -1.000000000000000000, 0.000000000000000000, 0.000000000000000000 ) ) ;
#4985 = EDGE_CURVE ( 'NONE', #17007, #8697, #17667, .T. ) ;
#4986 = DIRECTION ( 'NONE',  ( -1.000000000000000000, -0.000000000000000000, -0.000000000000000000 ) ) ;
#4987 = CARTESIAN_POINT ( 'NONE',  ( 1.491842756249030622, 7.499999999820669672, 14.00198125018031625 ) ) ;
#4988 = AXIS2_PLACEMENT_3D ( 'NONE', #1385, #4554, #20755 ) ;
#4989 = CARTESIAN_POINT ( 'NONE',  ( 1.343451552857795099E-09, 11.17563879731704723, 7.013640249713197328 ) ) ;
#4990 = AXIS2_PLACEMENT_3D ( 'NONE', #17891, #8228, #13213 ) ;
#4991 = DIRECTION ( 'NONE',  ( 1.000000000000000000, 0.000000000000000000, 0.000000000000000000 ) ) ;
#4992 = CARTESIAN_POINT ( 'NONE',  ( 85.00002539999999840, 0.000000000000000000, 0.000000000000000000 ) ) ;
#4993 = ORIENTED_EDGE ( 'NONE', *, *, #16242, .T. ) ;
#4994 = CIRCLE ( 'NONE', #1296, 2.649999999999999467 ) ;
#4995 = DIRECTION ( 'NONE',  ( -1.000000000000000000, 0.000000000000000000, -0.000000000000000000 ) ) ;
#4996 = CARTESIAN_POINT ( 'NONE',  ( 6.888301780572507305, -16.62983158603121936, 6.225737500180312800 ) ) ;
#4997 = CARTESIAN_POINT ( 'NONE',  ( 10.00000000000000178, -40.41646384503856382, 66.42520834682601105 ) ) ;
#4998 = VERTEX_POINT ( 'NONE', #13346 ) ;
#4999 = FACE_OUTER_BOUND ( 'NONE', #15942, .T. ) ;
#5000 = EDGE_LOOP ( 'NONE', ( #15911, #11132, #20497, #11180 ) ) ;
#5001 = CARTESIAN_POINT ( 'NONE',  ( 2.500000000000000000, -1.178949249685218748, -2.041999999999998039 ) ) ;
#5002 = CARTESIAN_POINT ( 'NONE',  ( 32.12996668197559558, -33.64348109762138961, -67.10678061411157103 ) ) ;
#5003 = ADVANCED_FACE ( 'NONE', ( #715 ), #7172, .T. ) ;
#5004 = ORIENTED_EDGE ( 'NONE', *, *, #4562, .T. ) ;
#5005 = AXIS2_PLACEMENT_3D ( 'NONE', #5230, #3632, #14504 ) ;
#5006 = ORIENTED_EDGE ( 'NONE', *, *, #14101, .T. ) ;
#5007 = CARTESIAN_POINT ( 'NONE',  ( 30.00000000000000000, -105.0000000000000000, -72.35596062816881613 ) ) ;
#5008 = TOROIDAL_SURFACE ( 'NONE', #3633, 10.79377999999999993, 0.06721999999999934972 ) ;
#5009 =( LENGTH_UNIT ( ) NAMED_UNIT ( * ) SI_UNIT ( .MILLI., .METRE. ) );
#5010 = LINE ( 'NONE', #14755, #6912 ) ;
#5011 = FACE_OUTER_BOUND ( 'NONE', #3070, .T. ) ;
#5012 = VERTEX_POINT ( 'NONE', #18627 ) ;
#5013 = CARTESIAN_POINT ( 'NONE',  ( -6.929096494179677101, -2.870125741905209527, 4.497237500180311542 ) ) ;
#5014 = CYLINDRICAL_SURFACE ( 'NONE', #14243, 65.24900000006525147 ) ;
#5015 = DIRECTION ( 'NONE',  ( -0.000000000000000000, -0.000000000000000000, -1.000000000000000000 ) ) ;
#5016 = DIRECTION ( 'NONE',  ( 1.000000000000000000, 0.000000000000000000, 0.000000000000000000 ) ) ;
#5017 = ORIENTED_EDGE ( 'NONE', *, *, #12781, .F. ) ;
#5018 = DIRECTION ( 'NONE',  ( -1.000000000000000000, -0.000000000000000000, -0.000000000000000000 ) ) ;
#5019 = ORIENTED_EDGE ( 'NONE', *, *, #16399, .T. ) ;
#5020 = CARTESIAN_POINT ( 'NONE',  ( -2.163827323447878234E-09, -18.00000000000000000, 14.33520000018031482 ) ) ;
#5021 = CARTESIAN_POINT ( 'NONE',  ( 0.000000000000000000, -64.80702306891100761, 7.581672767546201008 ) ) ;
#5022 = ORIENTED_EDGE ( 'NONE', *, *, #12228, .T. ) ;
#5023 = LINE ( 'NONE', #9586, #19408 ) ;
#5024 = ORIENTED_EDGE ( 'NONE', *, *, #14281, .T. ) ;
#5025 = DIRECTION ( 'NONE',  ( -1.000000000000000000, -0.000000000000000000, 0.000000000000000000 ) ) ;
#5026 = EDGE_CURVE ( 'NONE', #16083, #11557, #8505, .T. ) ;
#5027 = ORIENTED_EDGE ( 'NONE', *, *, #132, .T. ) ;
#5028 = DIRECTION ( 'NONE',  ( -0.000000000000000000, -0.000000000000000000, -1.000000000000000000 ) ) ;
#5029 = CARTESIAN_POINT ( 'NONE',  ( -31.74999999999995737, 5.204748896376250699E-16, -4.250000000000000000 ) ) ;
#5030 = CARTESIAN_POINT ( 'NONE',  ( -2.943691928843437999, -14.79893867722910450, -19.30892683115845543 ) ) ;
#5031 = ORIENTED_EDGE ( 'NONE', *, *, #3571, .T. ) ;
#5032 = DIRECTION ( 'NONE',  ( 0.000000000000000000, 0.000000000000000000, 1.000000000000000000 ) ) ;
#5033 = ORIENTED_EDGE ( 'NONE', *, *, #13131, .F. ) ;
#5034 = CARTESIAN_POINT ( 'NONE',  ( 50.00000000000000000, 4.299168419249266293, 84.99999999999998579 ) ) ;
#5035 = CARTESIAN_POINT ( 'NONE',  ( -18.00000000000000000, 2.163826221265758884E-09, 18.59605000018031262 ) ) ;
#5036 = CARTESIAN_POINT ( 'NONE',  ( 24.74873734152916072, 24.74873734152916072, -120.0000000000000142 ) ) ;
#5037 = DIRECTION ( 'NONE',  ( 0.000000000000000000, 0.000000000000000000, -1.000000000000000000 ) ) ;
#5038 = VERTEX_POINT ( 'NONE', #10054 ) ;
#5039 = DIRECTION ( 'NONE',  ( 0.000000000000000000, 0.000000000000000000, 1.000000000000000000 ) ) ;
#5040 = ORIENTED_EDGE ( 'NONE', *, *, #12921, .T. ) ;
#5041 = FILL_AREA_STYLE_COLOUR ( '', #1475 ) ;
#5042 = DIRECTION ( 'NONE',  ( 0.000000000000000000, 0.000000000000000000, -1.000000000000000000 ) ) ;
#5043 = ORIENTED_EDGE ( 'NONE', *, *, #15673, .F. ) ;
#5044 = DIRECTION ( 'NONE',  ( 0.000000000000000000, 0.000000000000000000, -1.000000000000000000 ) ) ;
#5045 = ADVANCED_FACE ( 'NONE', ( #8451 ), #14927, .F. ) ;
#5046 = ADVANCED_FACE ( 'NONE', ( #5274 ), #18216, .T. ) ;
#5047 = DIRECTION ( 'NONE',  ( 0.000000000000000000, 0.000000000000000000, 1.000000000000000000 ) ) ;
#5048 = PRODUCT_CONTEXT ( 'NONE', #2073, 'mechanical' ) ;
#5049 = CARTESIAN_POINT ( 'NONE',  ( -18.00000000043041481, -3.580422610670022987, -9.973481249819691641 ) ) ;
#5050 = ORIENTED_EDGE ( 'NONE', *, *, #19311, .F. ) ;
#5051 = LINE ( 'NONE', #1880, #11971 ) ;
#5052 = ADVANCED_FACE ( 'NONE', ( #16721 ), #8660, .F. ) ;
#5053 = DIRECTION ( 'NONE',  ( 1.000000000000000000, 0.000000000000000000, 0.000000000000000000 ) ) ;
#5054 = CARTESIAN_POINT ( 'NONE',  ( -12.54593441562640166, 8.382925371439625906, -12.55669816848092779 ) ) ;
#5055 = CARTESIAN_POINT ( 'NONE',  ( -17.50000000000000355, 0.000000000000000000, 43.00000000000000000 ) ) ;
#5056 = ORIENTED_EDGE ( 'NONE', *, *, #14047, .T. ) ;
#5057 = LINE ( 'NONE', #18604, #9901 ) ;
#5058 = CARTESIAN_POINT ( 'NONE',  ( -6.929096493489632635, 2.870125743571140919, 21.36526250018031803 ) ) ;
#5059 = FACE_OUTER_BOUND ( 'NONE', #15710, .T. ) ;
#5060 = VERTEX_POINT ( 'NONE', #15451 ) ;
#5061 = EDGE_CURVE ( 'NONE', #15524, #11465, #9194, .T. ) ;
#5062 = LINE ( 'NONE', #1891, #1124 ) ;
#5063 = ORIENTED_EDGE ( 'NONE', *, *, #9219, .F. ) ;
#5064 = DIRECTION ( 'NONE',  ( 0.000000000000000000, 0.000000000000000000, 1.000000000000000000 ) ) ;
#5065 = CARTESIAN_POINT ( 'NONE',  ( 10.19618095414378622, 15.25966316918061239, 19.93129375018031268 ) ) ;
#5066 = ORIENTED_EDGE ( 'NONE', *, *, #15321, .T. ) ;
#5067 = ORIENTED_EDGE ( 'NONE', *, *, #20293, .T. ) ;
#5068 = LINE ( 'NONE', #11344, #20541 ) ;
#5069 = EDGE_CURVE ( 'NONE', #16213, #14635, #12242, .T. ) ;
#5070 = EDGE_CURVE ( 'NONE', #7012, #15594, #20731, .T. ) ;
#5071 = DIRECTION ( 'NONE',  ( -1.000000000000000000, -0.000000000000000000, -0.000000000000000000 ) ) ;
#5072 = PRESENTATION_STYLE_ASSIGNMENT (( #1803 ) ) ;
#5073 = CARTESIAN_POINT ( 'NONE',  ( 30.00000000000000000, -105.0000000000000426, 77.45966692414833688 ) ) ;
#5075 = EDGE_CURVE ( 'NONE', #9398, #10361, #4646, .T. ) ;
#5074 = CARTESIAN_POINT ( 'NONE',  ( 0.000000000000000000, 38.69327817041845918, -52.53819777490596010 ) ) ;
#5076 = CARTESIAN_POINT ( 'NONE',  ( -6.929096494179684207, -2.870125741905212635, 10.76213750018031590 ) ) ;
#5077 = VECTOR ( 'NONE', #2566, 1000.000000000000000 ) ;
#5078 = CARTESIAN_POINT ( 'NONE',  ( -9.474249098604506258, -6.330490856366290053, 3.773796499713198305 ) ) ;
#5079 = PRODUCT_DEFINITION_SHAPE ( 'NONE', 'NONE',  #20957 ) ;
#5080 = DIRECTION ( 'NONE',  ( 0.000000000000000000, 0.000000000000000000, 1.000000000000000000 ) ) ;
#5081 = DIRECTION ( 'NONE',  ( 1.000000000000000000, -0.000000000000000000, -0.000000000000000000 ) ) ;
#5082 = ORIENTED_EDGE ( 'NONE', *, *, #3834, .T. ) ;
#5083 = CARTESIAN_POINT ( 'NONE',  ( 19.99999999999999645, -43.56693332842820610, 48.57318520917490190 ) ) ;
#5084 = AXIS2_PLACEMENT_3D ( 'NONE', #900, #7451, #10654 ) ;
#5085 = CARTESIAN_POINT ( 'NONE',  ( -18.00000000043041126, -3.580422610670022543, 18.30151875018031760 ) ) ;
#5086 = DIRECTION ( 'NONE',  ( 0.000000000000000000, -0.7308359642781300236, 0.6825531432186476843 ) ) ;
#5087 = EDGE_CURVE ( 'NONE', #4931, #20532, #17361, .T. ) ;
#5088 = ORIENTED_EDGE ( 'NONE', *, *, #1529, .F. ) ;
#5089 = EDGE_CURVE ( 'NONE', #18338, #14577, #11232, .T. ) ;
#5090 = CARTESIAN_POINT ( 'NONE',  ( 40.00000000000000711, -40.00000000000001421, -120.0000000000000142 ) ) ;
#5091 = ORIENTED_EDGE ( 'NONE', *, *, #19830, .T. ) ;
#5092 = DIRECTION ( 'NONE',  ( 1.000000000000000000, -0.000000000000000000, -0.000000000000000000 ) ) ;
#5093 = CARTESIAN_POINT ( 'NONE',  ( 43.13922815819793044, -11.21276953243446606, 82.40275014679680510 ) ) ;
#5094 = ORIENTED_EDGE ( 'NONE', *, *, #15068, .T. ) ;
#5095 = ORIENTED_EDGE ( 'NONE', *, *, #17544, .F. ) ;
#5096 = CARTESIAN_POINT ( 'NONE',  ( 0.000000000000000000, 10.74906464462118016, 71.19310085447973790 ) ) ;
#5097 = EDGE_CURVE ( 'NONE', #20910, #15314, #4798, .T. ) ;
#5098 = CARTESIAN_POINT ( 'NONE',  ( -15.15000000000000568, -3.245314017740485469E-16, -40.00000000000000000 ) ) ;
#5099 = CARTESIAN_POINT ( 'NONE',  ( 0.000000000000000000, -67.51707036274430607, 25.00890260772354523 ) ) ;
#5100 = VERTEX_POINT ( 'NONE', #14083 ) ;
#5101 = CARTESIAN_POINT ( 'NONE',  ( -5.303300859536631329, -5.303300858261583706, 13.33317500018031332 ) ) ;
#5102 = DIRECTION ( 'NONE',  ( 1.000000000000000000, 0.000000000000000000, 0.000000000000000000 ) ) ;
#5103 = CARTESIAN_POINT ( 'NONE',  ( -17.50000000000000355, 0.000000000000000000, 46.00000000000000711 ) ) ;
#5104 = DIRECTION ( 'NONE',  ( -1.000000000000000000, -0.000000000000000000, -0.000000000000000000 ) ) ;
#5105 = CARTESIAN_POINT ( 'NONE',  ( 19.99999999999999645, 0.000000000000000000, 0.000000000000000000 ) ) ;
#5106 = ORIENTED_EDGE ( 'NONE', *, *, #17189, .F. ) ;
#5107 = CARTESIAN_POINT ( 'NONE',  ( 16.62983158437509346, -6.888301784570739272, -23.22738749981969164 ) ) ;
#5108 = ORIENTED_EDGE ( 'NONE', *, *, #19311, .T. ) ;
#5109 = CARTESIAN_POINT ( 'NONE',  ( 18.00000000043041126, 3.580422610670019434, 21.10941875018031411 ) ) ;
#5110 = FACE_OUTER_BOUND ( 'NONE', #4586, .T. ) ;
#5111 = ORIENTED_EDGE ( 'NONE', *, *, #14896, .T. ) ;
#5112 = DIRECTION ( 'NONE',  ( -1.000000000000000000, -6.938893903907228378E-17, 0.000000000000000000 ) ) ;
#5113 = EDGE_LOOP ( 'NONE', ( #5452, #8295, #1006, #18242 ) ) ;
#5114 = CARTESIAN_POINT ( 'NONE',  ( 19.99999999999999645, -61.72688495901628869, 19.84591825363989415 ) ) ;
#5115 = CARTESIAN_POINT ( 'NONE',  ( 2.500000000000000000, 2.357898499370433054, -1.951563910473907981E-15 ) ) ;
#5116 = EDGE_LOOP ( 'NONE', ( #11366, #20273 ) ) ;
#5117 = AXIS2_PLACEMENT_3D ( 'NONE', #20722, #1144, #19046 ) ;
#5118 = AXIS2_PLACEMENT_3D ( 'NONE', #2002, #517, #12160 ) ;
#5119 = FACE_OUTER_BOUND ( 'NONE', #18132, .T. ) ;
#5120 = DIRECTION ( 'NONE',  ( 1.000000000000000000, 0.000000000000000000, 0.000000000000000000 ) ) ;
#5121 = TOROIDAL_SURFACE ( 'NONE', #14959, 10.79377999999999993, 0.06721999999999977993 ) ;
#5122 = CARTESIAN_POINT ( 'NONE',  ( -2.222972771497745192, -11.17563879704982632, 0.2933910006474270693 ) ) ;
#5123 = ADVANCED_FACE ( 'NONE', ( #2834 ), #3762, .T. ) ;
#5124 = ORIENTED_EDGE ( 'NONE', *, *, #13362, .T. ) ;
#5125 = CARTESIAN_POINT ( 'NONE',  ( -44.00000000000000000, -85.00000000000000000, -11.50000000000000711 ) ) ;
#5126 = EDGE_CURVE ( 'NONE', #1377, #20902, #5791, .T. ) ;
#5127 = CARTESIAN_POINT ( 'NONE',  ( 8.900000000000053646, 10.82531754730546147, 40.00000000000000000 ) ) ;
#5128 = ORIENTED_EDGE ( 'NONE', *, *, #12968, .T. ) ;
#5129 = AXIS2_PLACEMENT_3D ( 'NONE', #18930, #11282, #4396 ) ;
#5130 = FACE_OUTER_BOUND ( 'NONE', #610, .T. ) ;
#5131 = CIRCLE ( 'NONE', #8517, 39.99999999999999289 ) ;
#5132 = VERTEX_POINT ( 'NONE', #9095 ) ;
#5133 = CARTESIAN_POINT ( 'NONE',  ( 0.000000000000000000, 0.000000000000000000, 0.000000000000000000 ) ) ;
#5134 = AXIS2_PLACEMENT_3D ( 'NONE', #9527, #15997, #7947 ) ;
#5135 = CARTESIAN_POINT ( 'NONE',  ( 0.000000000000000000, -64.52323195238632536, 6.389157729492951354 ) ) ;
#5136 = CARTESIAN_POINT ( 'NONE',  ( 19.99999999999999645, 0.000000000000000000, 0.000000000000000000 ) ) ;
#5137 = ORIENTED_EDGE ( 'NONE', *, *, #7204, .T. ) ;
#5138 = CARTESIAN_POINT ( 'NONE',  ( 19.99999999999999645, -10.77748419466653651, -63.93680186330482940 ) ) ;
#5139 = EDGE_LOOP ( 'NONE', ( #15103, #16995, #18594, #10963 ) ) ;
#5140 =( NAMED_UNIT ( * ) PLANE_ANGLE_UNIT ( ) SI_UNIT ( $, .RADIAN. ) );
#5141 = CARTESIAN_POINT ( 'NONE',  ( -9.015947181032835626E-10, -7.500000000000007994, -19.28004999981968481 ) ) ;
#5142 = EDGE_LOOP ( 'NONE', ( #19295, #20826, #16444, #612 ) ) ;
#5143 = DIRECTION ( 'NONE',  ( 0.000000000000000000, 0.000000000000000000, -1.000000000000000000 ) ) ;
#5144 = VECTOR ( 'NONE', #16731, 1000.000000000000000 ) ;
#5145 = DIRECTION ( 'NONE',  ( 1.000000000000000000, 0.000000000000000000, 0.000000000000000000 ) ) ;
#5146 = VECTOR ( 'NONE', #2096, 1000.000000000000000 ) ;
#5147 = CARTESIAN_POINT ( 'NONE',  ( 13.67243654778935991, 5.663308646854338768, 24.57622941884154955 ) ) ;
#5148 = ORIENTED_EDGE ( 'NONE', *, *, #17056, .F. ) ;
#5149 = EDGE_CURVE ( 'NONE', #12516, #2692, #17337, .T. ) ;
#5150 = DIRECTION ( 'NONE',  ( -1.000000000000000000, 0.000000000000000000, -0.000000000000000000 ) ) ;
#5151 = DIRECTION ( 'NONE',  ( -0.000000000000000000, -0.000000000000000000, 1.000000000000000000 ) ) ;
#5152 = CARTESIAN_POINT ( 'NONE',  ( -12.54593441562640166, 8.382925371439625906, -3.131698168480926192 ) ) ;
#5153 = EDGE_LOOP ( 'NONE', ( #17444, #7861 ) ) ;
#5154 = VECTOR ( 'NONE', #19469, 1000.000000000000000 ) ;
#5155 = EDGE_CURVE ( 'NONE', #10337, #17904, #15765, .T. ) ;
#5156 = AXIS2_PLACEMENT_3D ( 'NONE', #13027, #6346, #7734 ) ;
#5157 = VERTEX_POINT ( 'NONE', #20427 ) ;
#5158 = STYLED_ITEM ( 'NONE', ( #17714 ), #10096 ) ;
#5159 = DIRECTION ( 'NONE',  ( -1.000000000000000000, 0.000000000000000000, 0.000000000000000000 ) ) ;
#5160 = CYLINDRICAL_SURFACE ( 'NONE', #17836, 2.649999999999999467 ) ;
#5161 = CYLINDRICAL_SURFACE ( 'NONE', #14138, 2.649999999999992806 ) ;
#5162 = CIRCLE ( 'NONE', #13306, 14.49999999999999467 ) ;
#5163 = VERTEX_POINT ( 'NONE', #7811 ) ;
#5164 = DIRECTION ( 'NONE',  ( 0.000000000000000000, 0.5195839500354290097, 0.8544194045464913456 ) ) ;
#5165 = ORIENTED_EDGE ( 'NONE', *, *, #13394, .T. ) ;
#5166 = DIRECTION ( 'NONE',  ( -1.000000000000000000, 0.000000000000000000, 0.000000000000000000 ) ) ;
#5167 = CARTESIAN_POINT ( 'NONE',  ( -10.19618095047497874, 15.25966317163202746, 18.16410625018031411 ) ) ;
#5168 = ORIENTED_EDGE ( 'NONE', *, *, #13304, .F. ) ;
#5169 = EDGE_CURVE ( 'NONE', #18530, #20075, #873, .T. ) ;
#5170 = ORIENTED_EDGE ( 'NONE', *, *, #16958, .F. ) ;
#5171 = PLANE ( 'NONE',  #19188 ) ;
#5172 = EDGE_CURVE ( 'NONE', #12906, #7841, #4325, .T. ) ;
#5173 = AXIS2_PLACEMENT_3D ( 'NONE', #18779, #12522, #4455 ) ;
#5174 = DIRECTION ( 'NONE',  ( 0.000000000000000000, 0.000000000000000000, 1.000000000000000000 ) ) ;
#5175 = CARTESIAN_POINT ( 'NONE',  ( 52.00000000000000000, -39.99999999999999289, 5.000000000000000000 ) ) ;
#5176 = DIRECTION ( 'NONE',  ( -1.000000000000000000, -0.000000000000000000, -0.000000000000000000 ) ) ;
#5177 = AXIS2_PLACEMENT_3D ( 'NONE', #18174, #16367, #6714 ) ;
#5178 = VECTOR ( 'NONE', #14671, 1000.000000000000000 ) ;
#5179 = DIRECTION ( 'NONE',  ( 0.000000000000000000, -0.8878852184023701133, -0.4600650377311617523 ) ) ;
#5180 = CARTESIAN_POINT ( 'NONE',  ( 2.870125743571140475, 6.929096493489632635, 23.72151250018031732 ) ) ;
#5181 = CARTESIAN_POINT ( 'NONE',  ( 11.17563879731704723, -1.343450868547281106E-09, 9.369890249713199282 ) ) ;
#5182 = AXIS2_PLACEMENT_3D ( 'NONE', #10306, #18461, #5626 ) ;
#5183 = CARTESIAN_POINT ( 'NONE',  ( 19.99999999999999645, -39.37110852956848817, 51.51683813304857296 ) ) ;
#5184 = LINE ( 'NONE', #319, #15442 ) ;
#5185 = AXIS2_PLACEMENT_3D ( 'NONE', #14817, #19473, #3263 ) ;
#5186 = EDGE_CURVE ( 'NONE', #12410, #1870, #2214, .T. ) ;
#5187 = ORIENTED_EDGE ( 'NONE', *, *, #12888, .F. ) ;
#5188 = DIRECTION ( 'NONE',  ( 0.000000000000000000, 0.7308359642781254717, -0.6825531432186525693 ) ) ;
#5189 = EDGE_CURVE ( 'NONE', #520, #1320, #14861, .T. ) ;
#5190 = CARTESIAN_POINT ( 'NONE',  ( 18.00000000043041126, 3.580422610670019434, 13.58901875018031369 ) ) ;
#5191 = LINE ( 'NONE', #8377, #13021 ) ;
#5192 = VECTOR ( 'NONE', #6070, 1000.000000000000000 ) ;
#5193 = ORIENTED_EDGE ( 'NONE', *, *, #19576, .F. ) ;
#5194 = VECTOR ( 'NONE', #12089, 1000.000000000000000 ) ;
#5195 = CYLINDRICAL_SURFACE ( 'NONE', #17686, 2.649999999999999467 ) ;
#5196 = VERTEX_POINT ( 'NONE', #9619 ) ;
#5197 = LINE ( 'NONE', #19716, #18303 ) ;
#5198 = LINE ( 'NONE', #4898, #8677 ) ;
#5199 = EDGE_CURVE ( 'NONE', #4685, #14887, #19477, .T. ) ;
#5200 = ORIENTED_EDGE ( 'NONE', *, *, #7570, .T. ) ;
#5201 =( REPRESENTATION_RELATIONSHIP ('NONE','NONE', #13739, #2344 ) REPRESENTATION_RELATIONSHIP_WITH_TRANSFORMATION ( #15856 )SHAPE_REPRESENTATION_RELATIONSHIP( ) );
#5202 = EDGE_CURVE ( 'NONE', #14849, #5544, #17815, .T. ) ;
#5203 = ORIENTED_EDGE ( 'NONE', *, *, #7961, .F. ) ;
#5204 = CARTESIAN_POINT ( 'NONE',  ( 19.99999999999999645, 46.17500197033056963, 55.24372537266411598 ) ) ;
#5205 = AXIS2_PLACEMENT_3D ( 'NONE', #12443, #14462, #17629 ) ;
#5206 =( NAMED_UNIT ( * ) PLANE_ANGLE_UNIT ( ) SI_UNIT ( $, .RADIAN. ) );
#5207 = DIRECTION ( 'NONE',  ( -1.000000000000000000, 0.000000000000000000, 0.000000000000000000 ) ) ;
#5208 = CIRCLE ( 'NONE', #4535, 27.60000000002760245 ) ;
#5209 = LINE ( 'NONE', #14756, #4190 ) ;
#5210 = EDGE_CURVE ( 'NONE', #4467, #4451, #11205, .T. ) ;
#5211 = AXIS2_PLACEMENT_3D ( 'NONE', #16868, #15071, #10619 ) ;
#5212 = ADVANCED_FACE ( 'NONE', ( #1574 ), #11506, .T. ) ;
#5213 = AXIS2_PLACEMENT_3D ( 'NONE', #5224, #19432, #3329 ) ;
#5214 = CARTESIAN_POINT ( 'NONE',  ( -5.303300858261583706, 5.303300859536630441, 6.264425000180311010 ) ) ;
#5215 = CARTESIAN_POINT ( 'NONE',  ( 0.000000000000000000, 0.000000000000000000, -5.599999999999999645 ) ) ;
#5216 = CARTESIAN_POINT ( 'NONE',  ( 50.00000000000000000, 36.35083268962920044, -90.00000000000000000 ) ) ;
#5217 = CARTESIAN_POINT ( 'NONE',  ( -49.35000000000000142, -99.99999999999998579, 5.000000000000000000 ) ) ;
#5218 = CYLINDRICAL_SURFACE ( 'NONE', #1828, 2.500000000000000444 ) ;
#5219 = ORIENTED_EDGE ( 'NONE', *, *, #1851, .F. ) ;
#5220 = DIRECTION ( 'NONE',  ( 0.000000000000000000, -1.541976423090495387E-16, 1.000000000000000000 ) ) ;
#5221 = EDGE_CURVE ( 'NONE', #13702, #19113, #3047, .T. ) ;
#5222 = VERTEX_POINT ( 'NONE', #17888 ) ;
#5223 = CARTESIAN_POINT ( 'NONE',  ( 6.888301780572507305, -16.62983158603121936, 13.74613750018031588 ) ) ;
#5224 = CARTESIAN_POINT ( 'NONE',  ( -6.232800000000000118, 0.000000000000000000, 0.000000000000000000 ) ) ;
#5225 = CIRCLE ( 'NONE', #7239, 8.500000000000000000 ) ;
#5226 = ORIENTED_EDGE ( 'NONE', *, *, #13261, .F. ) ;
#5227 = DIRECTION ( 'NONE',  ( 0.000000000000000000, 1.000000000000000000, -1.224646799147353207E-16 ) ) ;
#5228 = EDGE_LOOP ( 'NONE', ( #17305, #8839, #20327, #2572, #9641, #6143 ) ) ;
#5229 = CARTESIAN_POINT ( 'NONE',  ( 50.00000000000000000, 36.35083268962917202, 90.00000000000000000 ) ) ;
#5230 = CARTESIAN_POINT ( 'NONE',  ( -6.679999999999996163, -11.17999999999998906, 1.369155121446740171E-15 ) ) ;
#5231 = ORIENTED_EDGE ( 'NONE', *, *, #20217, .F. ) ;
#5232 = CIRCLE ( 'NONE', #9294, 2.649999999999994582 ) ;
#5233 = CARTESIAN_POINT ( 'NONE',  ( 19.99999999999999645, 61.72688495901613948, -19.84591825364033468 ) ) ;
#5234 = CARTESIAN_POINT ( 'NONE',  ( -7.632783294297951215E-14, -4.618802153517020948, -0.3572655899081733644 ) ) ;
#5235 = DIRECTION ( 'NONE',  ( 1.000000000000000000, 0.000000000000000000, 0.000000000000000000 ) ) ;
#5236 = PRESENTATION_LAYER_ASSIGNMENT (  '', '', ( #20852 ) ) ;
#5237 = CARTESIAN_POINT ( 'NONE',  ( -11.17563879704982988, 2.222972771497744748, 12.07464100064743029 ) ) ;
#5238 = VERTEX_POINT ( 'NONE', #20843 ) ;
#5239 = EDGE_CURVE ( 'NONE', #9794, #16683, #13408, .T. ) ;
#5240 = CARTESIAN_POINT ( 'NONE',  ( -24.99999999999999289, -160.0000000000000000, -53.99496054166690584 ) ) ;
#5241 = DIRECTION ( 'NONE',  ( 0.000000000000000000, 0.000000000000000000, 1.000000000000000000 ) ) ;
#5242 = EDGE_LOOP ( 'NONE', ( #13007, #14834, #10313, #11825 ) ) ;
#5243 = DIRECTION ( 'NONE',  ( -1.000000000000000000, 0.000000000000000000, 0.000000000000000000 ) ) ;
#5244 = AXIS2_PLACEMENT_3D ( 'NONE', #17966, #19447, #9903 ) ;
#5245 = ORIENTED_EDGE ( 'NONE', *, *, #20626, .T. ) ;
#5246 = CARTESIAN_POINT ( 'NONE',  ( -15.25966316918061771, 10.19618095414378622, 10.05464375018031475 ) ) ;
#5247 = DIRECTION ( 'NONE',  ( 0.000000000000000000, 0.000000000000000000, -1.000000000000000000 ) ) ;
#5248 = FACE_OUTER_BOUND ( 'NONE', #18113, .T. ) ;
#5249 = VERTEX_POINT ( 'NONE', #3352 ) ;
#5250 = FACE_OUTER_BOUND ( 'NONE', #17449, .T. ) ;
#5251 = DIRECTION ( 'NONE',  ( 1.000000000000000000, 0.000000000000000000, 0.000000000000000000 ) ) ;
#5252 = ORIENTED_EDGE ( 'NONE', *, *, #1853, .T. ) ;
#5253 = DIRECTION ( 'NONE',  ( -0.000000000000000000, -0.000000000000000000, 1.000000000000000000 ) ) ;
#5254 = ADVANCED_FACE ( 'NONE', ( #8123 ), #17980, .T. ) ;
#5255 = ORIENTED_EDGE ( 'NONE', *, *, #9082, .F. ) ;
#5256 = DIRECTION ( 'NONE',  ( 0.000000000000000000, 0.000000000000000000, 1.000000000000000000 ) ) ;
#5257 = AXIS2_PLACEMENT_3D ( 'NONE', #17314, #15510, #2791 ) ;
#5258 = PRODUCT_DEFINITION_SHAPE ( 'NONE', 'NONE',  #17526 ) ;
#5259 = DIRECTION ( 'NONE',  ( -0.000000000000000000, 0.000000000000000000, -1.000000000000000000 ) ) ;
#5260 = SHAPE_DEFINITION_REPRESENTATION ( #697, #7225 ) ;
#5261 = CARTESIAN_POINT ( 'NONE',  ( -2.943691928843437999, -14.79893867722910450, 18.39107316884155097 ) ) ;
#5262 = ORIENTED_EDGE ( 'NONE', *, *, #17899, .F. ) ;
#5263 = CARTESIAN_POINT ( 'NONE',  ( 19.99999999999999645, -56.42118728228132341, -32.77318456705499017 ) ) ;
#5264 = CARTESIAN_POINT ( 'NONE',  ( 10.46442989202483531, -10.46442989454075168, -16.97466691848093134 ) ) ;
#5265 = AXIS2_PLACEMENT_3D ( 'NONE', #2894, #3002, #15823 ) ;
#5266 = ORIENTED_EDGE ( 'NONE', *, *, #12844, .T. ) ;
#5267 = AXIS2_PLACEMENT_3D ( 'NONE', #15050, #13251, #3594 ) ;
#5268 = ORIENTED_EDGE ( 'NONE', *, *, #14560, .F. ) ;
#5269 = CARTESIAN_POINT ( 'NONE',  ( 36.56410540690647792, -119.8383876564256809, 84.69420751047145757 ) ) ;
#5270 = CARTESIAN_POINT ( 'NONE',  ( 7.500000000179340987, 1.491842754445842134, 18.92926875018030941 ) ) ;
#5271 = ORIENTED_EDGE ( 'NONE', *, *, #11130, .T. ) ;
#5272 = CARTESIAN_POINT ( 'NONE',  ( 5.303300858261588147, -5.303300859536636658, 7.816825000180313232 ) ) ;
#5273 = VERTEX_POINT ( 'NONE', #6327 ) ;
#5274 = FACE_OUTER_BOUND ( 'NONE', #9226, .T. ) ;
#5275 = CARTESIAN_POINT ( 'NONE',  ( 6.888301780572505528, -16.62983158603121581, 13.74613750018031233 ) ) ;
#5276 = EDGE_CURVE ( 'NONE', #4175, #7756, #6527, .T. ) ;
#5277 = VERTEX_POINT ( 'NONE', #19358 ) ;
#5278 = ORIENTED_EDGE ( 'NONE', *, *, #11450, .T. ) ;
#5279 = DIRECTION ( 'NONE',  ( -1.000000000000000000, -0.000000000000000000, 0.000000000000000000 ) ) ;
#5280 = AXIS2_PLACEMENT_3D ( 'NONE', #5827, #15264, #18777 ) ;
#5281 = CYLINDRICAL_SURFACE ( 'NONE', #1253, 72.00000000007199219 ) ;
#5282 = CARTESIAN_POINT ( 'NONE',  ( 19.99999999999999645, -45.48683723007179225, -46.78012013466265273 ) ) ;
#5283 = CARTESIAN_POINT ( 'NONE',  ( -5.303300858261589035, 5.303300859536635770, -15.74567499981968588 ) ) ;
#5284 = EDGE_CURVE ( 'NONE', #13416, #3271, #17579, .T. ) ;
#5285 = AXIS2_PLACEMENT_3D ( 'NONE', #20919, #4712, #1234 ) ;
#5286 = CIRCLE ( 'NONE', #14765, 65.24900000006525147 ) ;
#5287 = CARTESIAN_POINT ( 'NONE',  ( 6.249999999999902300, -10.82531754730554496, 46.00000000000000711 ) ) ;
#5288 = CARTESIAN_POINT ( 'NONE',  ( -5.303300858261589035, 5.303300859536635770, -6.320674999819683393 ) ) ;
#5289 = CARTESIAN_POINT ( 'NONE',  ( -1.343452921478823292E-09, -11.17563879731704723, -16.54885975028680889 ) ) ;
#5290 = CIRCLE ( 'NONE', #5619, 2.041999999999999815 ) ;
#5291 = DIRECTION ( 'NONE',  ( 1.000000000000000000, 0.000000000000000000, 0.000000000000000000 ) ) ;
#5292 = DIRECTION ( 'NONE',  ( 1.000000000000000000, 0.000000000000000000, 0.000000000000000000 ) ) ;
#5293 = CIRCLE ( 'NONE', #14825, 11.50000000000000000 ) ;
#5294 = ORIENTED_EDGE ( 'NONE', *, *, #13484, .F. ) ;
#5295 = LINE ( 'NONE', #18129, #18704 ) ;
#5296 = AXIS2_PLACEMENT_3D ( 'NONE', #11449, #1608, #2194 ) ;
#5297 = CARTESIAN_POINT ( 'NONE',  ( -12.72792205982779912, 12.72792206288790950, -8.500824999819686312 ) ) ;
#5298 = CARTESIAN_POINT ( 'NONE',  ( -65.00002539999999840, 5.400000000000000355, 1.000000000000000000 ) ) ;
#5299 = ORIENTED_EDGE ( 'NONE', *, *, #6455, .T. ) ;
#5300 = LINE ( 'NONE', #3803, #5194 ) ;
#5301 = ORIENTED_EDGE ( 'NONE', *, *, #14264, .F. ) ;
#5302 = DIRECTION ( 'NONE',  ( 0.000000000000000000, 0.000000000000000000, -1.000000000000000000 ) ) ;
#5303 = PLANE ( 'NONE',  #9025 ) ;
#5304 = EDGE_LOOP ( 'NONE', ( #11435, #16240, #7271, #18294, #4348, #11997 ) ) ;
#5305 = ORIENTED_EDGE ( 'NONE', *, *, #548, .F. ) ;
#5306 = DIRECTION ( 'NONE',  ( 0.000000000000000000, 0.000000000000000000, 1.000000000000000000 ) ) ;
#5307 = CIRCLE ( 'NONE', #19868, 2.099999999999999645 ) ;
#5308 = CARTESIAN_POINT ( 'NONE',  ( -65.00002539999999840, 0.000000000000000000, 0.000000000000000000 ) ) ;
#5309 = EDGE_CURVE ( 'NONE', #17187, #17770, #15426, .T. ) ;
#5310 = CIRCLE ( 'NONE', #20556, 27.60000000002759535 ) ;
#5311 = EDGE_CURVE ( 'NONE', #8808, #17307, #16280, .T. ) ;
#5312 = CARTESIAN_POINT ( 'NONE',  ( 0.000000000000000000, -11.98658579560631843, 64.13855129306463709 ) ) ;
#5313 = AXIS2_PLACEMENT_3D ( 'NONE', #8424, #16581, #15504 ) ;
#5314 = CARTESIAN_POINT ( 'NONE',  ( 4.248408730893245888, 6.358192987158590270, 8.326143750180312608 ) ) ;
#5315 = CONICAL_SURFACE ( 'NONE', #11088, 4.000000000000000000, 1.047197551196595855 ) ;
#5316 = CARTESIAN_POINT ( 'NONE',  ( -23.00000000000000000, 2.816687638038912352E-15, -120.0000000000000142 ) ) ;
#5317 = ADVANCED_FACE ( 'NONE', ( #6422 ), #4843, .F. ) ;
#5318 = DIRECTION ( 'NONE',  ( -1.000000000000000000, 0.000000000000000000, 0.000000000000000000 ) ) ;
#5319 = CARTESIAN_POINT ( 'NONE',  ( -4.000000000000000000, -2.309401076758531346, -0.3572655899081733644 ) ) ;
#5320 = ORIENTED_EDGE ( 'NONE', *, *, #7082, .F. ) ;
#5321 = CARTESIAN_POINT ( 'NONE',  ( 4.248408730893249441, 6.358192987158596488, 5.166043750180316252 ) ) ;
#5322 = ORIENTED_EDGE ( 'NONE', *, *, #7665, .T. ) ;
#5323 = DIRECTION ( 'NONE',  ( 1.000000000000000000, 0.000000000000000000, 0.000000000000000000 ) ) ;
#5324 = CARTESIAN_POINT ( 'NONE',  ( -11.54691128655044352, -18.15138880902594565, 72.10074112616622699 ) ) ;
#5325 = CIRCLE ( 'NONE', #5005, 0.3200000000000008393 ) ;
#5326 = VERTEX_POINT ( 'NONE', #17785 ) ;
#5327 = CARTESIAN_POINT ( 'NONE',  ( 19.99999999999999645, -19.38316218894168586, -61.87375713201008409 ) ) ;
#5328 = ORIENTED_EDGE ( 'NONE', *, *, #18851, .T. ) ;
#5329 = DIRECTION ( 'NONE',  ( 0.000000000000000000, -0.000000000000000000, 1.000000000000000000 ) ) ;
#5330 = DIRECTION ( 'NONE',  ( 0.000000000000000000, 0.5195839500354345608, -0.8544194045464879039 ) ) ;
#5331 = AXIS2_PLACEMENT_3D ( 'NONE', #2505, #19143, #5892 ) ;
#5332 = VERTEX_POINT ( 'NONE', #8225 ) ;
#5333 = EDGE_CURVE ( 'NONE', #19867, #12993, #17798, .T. ) ;
#5334 = DIRECTION ( 'NONE',  ( 0.000000000000000000, 0.000000000000000000, -1.000000000000000000 ) ) ;
#5335 = CARTESIAN_POINT ( 'NONE',  ( -17.99999999956958163, 3.580422614997673669, -1.864018749819690957 ) ) ;
#5336 = EDGE_CURVE ( 'NONE', #8404, #13162, #18465, .T. ) ;
#5337 = EDGE_CURVE ( 'NONE', #8415, #19935, #3944, .T. ) ;
#5338 = DIRECTION ( 'NONE',  ( -1.000000000000000000, 0.000000000000000000, -0.000000000000000000 ) ) ;
#5339 = CARTESIAN_POINT ( 'NONE',  ( -10.32494394809439875, -4.276731812588566051, 11.19104725064742745 ) ) ;
#5340 = EDGE_LOOP ( 'NONE', ( #9730, #6806 ) ) ;
#5342 = ADVANCED_FACE ( 'NONE', ( #17100 ), #13599, .T. ) ;
#5341 = DIRECTION ( 'NONE',  ( -1.000000000000000000, 0.000000000000000000, -0.000000000000000000 ) ) ;
#5343 = CARTESIAN_POINT ( 'NONE',  ( -30.00000000000000000, -85.00000000000000000, -1.040949779275250179E-14 ) ) ;
#5344 = ORIENTED_EDGE ( 'NONE', *, *, #4709, .T. ) ;
#5345 = CYLINDRICAL_SURFACE ( 'NONE', #9808, 10.85999999999999410 ) ;
#5346 = EDGE_LOOP ( 'NONE', ( #4689, #11571, #7382, #8286 ) ) ;
#5347 = CARTESIAN_POINT ( 'NONE',  ( 3.580422610670020322, -18.00000000043041126, 6.520268750180314932 ) ) ;
#5348 = LINE ( 'NONE', #19764, #9021 ) ;
#5349 = LINE ( 'NONE', #9911, #19172 ) ;
#5350 = VERTEX_POINT ( 'NONE', #13923 ) ;
#5351 = FACE_OUTER_BOUND ( 'NONE', #17125, .T. ) ;
#5352 = VERTEX_POINT ( 'NONE', #3553 ) ;
#5353 = SURFACE_SIDE_STYLE ('',( #1768 ) ) ;
#5354 = EDGE_CURVE ( 'NONE', #939, #2292, #545, .T. ) ;
#5355 = EDGE_CURVE ( 'NONE', #6711, #12516, #20836, .T. ) ;
#5356 = ORIENTED_EDGE ( 'NONE', *, *, #2902, .T. ) ;
#5357 = LINE ( 'NONE', #498, #2619 ) ;
#5358 = EDGE_CURVE ( 'NONE', #5467, #19615, #12333, .T. ) ;
#5359 = CARTESIAN_POINT ( 'NONE',  ( 6.359999999999995879, 10.85999999999999943, 0.000000000000000000 ) ) ;
#5360 = ITEM_DEFINED_TRANSFORMATION ( 'NONE', 'NONE', #18102,  #12461 ) ;
#5361 = CARTESIAN_POINT ( 'NONE',  ( 2.943691928843431782, 14.79893867722910628, 13.67857316884154706 ) ) ;
#5362 = ORIENTED_EDGE ( 'NONE', *, *, #4320, .T. ) ;
#5363 = DIRECTION ( 'NONE',  ( 0.000000000000000000, 0.000000000000000000, 1.000000000000000000 ) ) ;
#5364 = ORIENTED_EDGE ( 'NONE', *, *, #17387, .F. ) ;
#5365 = FACE_BOUND ( 'NONE', #5953, .T. ) ;
#5366 = CARTESIAN_POINT ( 'NONE',  ( -16.62983158437509701, 6.888301784570728614, 17.28051250018031126 ) ) ;
#5367 = EDGE_CURVE ( 'NONE', #10658, #7264, #18588, .T. ) ;
#5368 = LINE ( 'NONE', #2401, #11227 ) ;
#5369 = AXIS2_PLACEMENT_3D ( 'NONE', #20468, #5946, #7426 ) ;
#5370 = ORIENTED_EDGE ( 'NONE', *, *, #8651, .F. ) ;
#5371 = CARTESIAN_POINT ( 'NONE',  ( 32.39354794939547588, -114.5261895919207120, 81.05644908113433189 ) ) ;
#5372 = CARTESIAN_POINT ( 'NONE',  ( -1.321505333908964186, 3.855830693249140850, -5.565789719053469753 ) ) ;
#5373 = ORIENTED_EDGE ( 'NONE', *, *, #4699, .F. ) ;
#5374 = CARTESIAN_POINT ( 'NONE',  ( -7.500000000000007105, -3.289131931996631318E-15, 11.35120000000231677 ) ) ;
#5375 = ORIENTED_EDGE ( 'NONE', *, *, #7907, .F. ) ;
#5376 = DIRECTION ( 'NONE',  ( -1.000000000000000000, 0.000000000000000000, 0.000000000000000000 ) ) ;
#5377 = CARTESIAN_POINT ( 'NONE',  ( -15.25966317163202923, -10.19618095047497874, -3.042143749819689713 ) ) ;
#5378 = ORIENTED_EDGE ( 'NONE', *, *, #8570, .T. ) ;
#5379 = ORIENTED_EDGE ( 'NONE', *, *, #6877, .T. ) ;
#5380 = CARTESIAN_POINT ( 'NONE',  ( 10.00000000000000178, -164.9999999999999716, 66.80000000000001137 ) ) ;
#5381 = LINE ( 'NONE', #10267, #9710 ) ;
#5382 = CARTESIAN_POINT ( 'NONE',  ( -24.99999999999999289, 31.35083268962915426, -50.63110039191615641 ) ) ;
#5383 = CYLINDRICAL_SURFACE ( 'NONE', #17739, 72.00000000007199219 ) ;
#5384 = UNCERTAINTY_MEASURE_WITH_UNIT (LENGTH_MEASURE( 1.000000000000000082E-05 ), #6360, 'distance_accuracy_value', 'NONE');
#5385 = DIRECTION ( 'NONE',  ( 1.000000000000000000, 1.836909530733573776E-16, 0.000000000000000000 ) ) ;
#5386 = CARTESIAN_POINT ( 'NONE',  ( 1.491842756249030622, 7.499999999820669672, -4.848018749819687834 ) ) ;
#5387 = EDGE_CURVE ( 'NONE', #15031, #9320, #14077, .T. ) ;
#5388 = CARTESIAN_POINT ( 'NONE',  ( -9.474249097082497073, 6.330490858644137298, -13.30901600028680321 ) ) ;
#5389 = EDGE_CURVE ( 'NONE', #18397, #297, #16433, .T. ) ;
#5390 = DIRECTION ( 'NONE',  ( -1.000000000000000000, -0.000000000000000000, -0.000000000000000000 ) ) ;
#5391 = CARTESIAN_POINT ( 'NONE',  ( 19.99999999999999645, 0.000000000000000000, 0.000000000000000000 ) ) ;
#5392 = ORIENTED_EDGE ( 'NONE', *, *, #6286, .T. ) ;
#5393 = DIRECTION ( 'NONE',  ( -1.000000000000000000, 0.000000000000000000, -0.000000000000000000 ) ) ;
#5394 = CARTESIAN_POINT ( 'NONE',  ( 12.72792206288790950, 12.72792205982780089, -6.144574999819688799 ) ) ;
#5395 = DIRECTION ( 'NONE',  ( 1.000000000000000000, 0.000000000000000000, 0.000000000000000000 ) ) ;
#5396 = VERTEX_POINT ( 'NONE', #6832 ) ;
#5397 = DIRECTION ( 'NONE',  ( -1.000000000000000000, 0.000000000000000000, 0.000000000000000000 ) ) ;
#5398 = CIRCLE ( 'NONE', #17266, 20.00000000000000000 ) ;
#5399 = ORIENTED_EDGE ( 'NONE', *, *, #7137, .T. ) ;
#5400 = CARTESIAN_POINT ( 'NONE',  ( 50.00000000000000000, -164.9999999999999716, -90.00000000000001421 ) ) ;
#5401 = CARTESIAN_POINT ( 'NONE',  ( -21.50000000000000000, 0.000000000000000000, -68.00000000000000000 ) ) ;
#5402 = VERTEX_POINT ( 'NONE', #18088 ) ;
#5403 = ORIENTED_EDGE ( 'NONE', *, *, #4453, .T. ) ;
#5404 = CARTESIAN_POINT ( 'NONE',  ( 8.500000000000000000, 1.040949779275250140E-15, -81.99999999999998579 ) ) ;
#5405 = DIRECTION ( 'NONE',  ( 1.000000000000000000, -0.000000000000000000, -0.000000000000000000 ) ) ;
#5406 = LINE ( 'NONE', #18348, #3508 ) ;
#5407 = CARTESIAN_POINT ( 'NONE',  ( 4.248408730893245888, 6.358192987158590270, -1.098856249819687880 ) ) ;
#5408 = VECTOR ( 'NONE', #652, 1000.000000000000000 ) ;
#5409 = CARTESIAN_POINT ( 'NONE',  ( 32.40156131938952200, -114.5405781163270689, -81.06459374562506071 ) ) ;
#5410 = CARTESIAN_POINT ( 'NONE',  ( -40.00000000000000000, 29.99999999999999289, -120.0000000000000142 ) ) ;
#5411 = DIRECTION ( 'NONE',  ( 0.000000000000000000, -1.287488025362403787E-15, -1.000000000000000000 ) ) ;
#5412 = DIRECTION ( 'NONE',  ( 0.000000000000000000, 0.000000000000000000, -1.000000000000000000 ) ) ;
#5413 = VERTEX_POINT ( 'NONE', #18477 ) ;
#5414 = CARTESIAN_POINT ( 'NONE',  ( 2.500000000000000000, 1.178949249685217415, 2.041999999999998483 ) ) ;
#5415 = ORIENTED_EDGE ( 'NONE', *, *, #17475, .T. ) ;
#5416 = CARTESIAN_POINT ( 'NONE',  ( -17.99999999956958519, 3.580422614997674113, -1.864018749819687404 ) ) ;
#5417 = LINE ( 'NONE', #568, #4219 ) ;
#5418 = AXIS2_PLACEMENT_3D ( 'NONE', #19624, #9985, #18248 ) ;
#5419 = ORIENTED_EDGE ( 'NONE', *, *, #10012, .T. ) ;
#5420 = EDGE_CURVE ( 'NONE', #20609, #3307, #3942, .T. ) ;
#5421 = DIRECTION ( 'NONE',  ( -1.000000000000000000, 0.000000000000000000, 0.000000000000000000 ) ) ;
#5422 = ORIENTED_EDGE ( 'NONE', *, *, #13798, .T. ) ;
#5423 = PRODUCT_DEFINITION_SHAPE ( 'NONE', 'NONE',  #20960 ) ;
#5424 = CARTESIAN_POINT ( 'NONE',  ( 45.76122707727121508, -127.3290820621008947, 85.00000000000000000 ) ) ;
#5425 = DIRECTION ( 'NONE',  ( -0.000000000000000000, -0.000000000000000000, -1.000000000000000000 ) ) ;
#5426 = ORIENTED_EDGE ( 'NONE', *, *, #9500, .T. ) ;
#5427 = CARTESIAN_POINT ( 'NONE',  ( -1.491842754445841690, 7.500000000179340987, -11.70198124981969201 ) ) ;
#5428 = CARTESIAN_POINT ( 'NONE',  ( -2.163827323447877821E-09, -17.99999999999999645, -13.93979999981969442 ) ) ;
#5429 = CARTESIAN_POINT ( 'NONE',  ( 50.00000000000000000, 36.35083268962915781, 50.00000000000000000 ) ) ;
#5430 = ADVANCED_FACE ( 'NONE', ( #12220, #16889 ), #2364, .T. ) ;
#5431 = DIRECTION ( 'NONE',  ( -0.000000000000000000, -0.000000000000000000, -1.000000000000000000 ) ) ;
#5432 = VECTOR ( 'NONE', #5329, 1000.000000000000000 ) ;
#5433 = CARTESIAN_POINT ( 'NONE',  ( -7.902369976724401113, 7.902369978624329327, 3.533234750647429312 ) ) ;
#5434 = ORIENTED_EDGE ( 'NONE', *, *, #288, .T. ) ;
#5435 = DIRECTION ( 'NONE',  ( 0.000000000000000000, 0.000000000000000000, -1.000000000000000000 ) ) ;
#5436 = DIRECTION ( 'NONE',  ( 0.000000000000000000, -0.5000000000000011102, -0.8660254037844379305 ) ) ;
#5437 = VERTEX_POINT ( 'NONE', #5643 ) ;
#5438 = CARTESIAN_POINT ( 'NONE',  ( 10.15192380093073332, -18.95599582743659184, -71.71153801002554928 ) ) ;
#5439 = VERTEX_POINT ( 'NONE', #7340 ) ;
#5440 = CARTESIAN_POINT ( 'NONE',  ( 16.62983158437509346, -6.888301784570739272, 5.047612500180314044 ) ) ;
#5441 = CARTESIAN_POINT ( 'NONE',  ( 19.99999999999999645, 58.26603306962021378, -42.29739224042413070 ) ) ;
#5442 = DIRECTION ( 'NONE',  ( -1.648349939164583742E-16, 1.000000000000000000, 0.000000000000000000 ) ) ;
#5443 = ORIENTED_EDGE ( 'NONE', *, *, #15716, .F. ) ;
#5444 = ADVANCED_FACE ( 'NONE', ( #12120 ), #16983, .T. ) ;
#5445 = ORIENTED_EDGE ( 'NONE', *, *, #2623, .T. ) ;
#5446 = CARTESIAN_POINT ( 'NONE',  ( 9.000000000000007105, -85.00000000000000000, 0.000000000000000000 ) ) ;
#5447 = ADVANCED_FACE ( 'NONE', ( #5745 ), #18687, .F. ) ;
#5448 = CIRCLE ( 'NONE', #3089, 2.055000000000000160 ) ;
#5449 = VERTEX_POINT ( 'NONE', #2787 ) ;
#5450 = DIRECTION ( 'NONE',  ( 0.000000000000000000, 0.000000000000000000, -1.000000000000000000 ) ) ;
#5451 = EDGE_CURVE ( 'NONE', #5249, #18498, #20591, .T. ) ;
#5452 = ORIENTED_EDGE ( 'NONE', *, *, #2647, .F. ) ;
#5453 = AXIS2_PLACEMENT_3D ( 'NONE', #4680, #3298, #11241 ) ;
#5454 = LINE ( 'NONE', #11726, #17867 ) ;
#5455 = DIRECTION ( 'NONE',  ( 0.000000000000000000, 0.000000000000000000, 1.000000000000000000 ) ) ;
#5456 = CARTESIAN_POINT ( 'NONE',  ( 13.67243654642775574, -5.663308650141541278, 16.32935441884154315 ) ) ;
#5458 = ORIENTED_EDGE ( 'NONE', *, *, #1193, .F. ) ;
#5457 = AXIS2_PLACEMENT_3D ( 'NONE', #6463, #8165, #17830 ) ;
#5459 = DIRECTION ( 'NONE',  ( -1.000000000000000000, -0.000000000000000000, 0.000000000000000000 ) ) ;
#5460 = AXIS2_PLACEMENT_3D ( 'NONE', #10794, #10691, #9302 ) ;
#5461 = EDGE_CURVE ( 'NONE', #10995, #7518, #11257, .T. ) ;
#5462 = CARTESIAN_POINT ( 'NONE',  ( -9.651484534775427448, -19.22442619234774241, 77.16801304840511477 ) ) ;
#5463 = EDGE_CURVE ( 'NONE', #857, #254, #14353, .T. ) ;
#5464 = CARTESIAN_POINT ( 'NONE',  ( -8.382925371439625906, -12.54593441562639988, -14.91294816848093063 ) ) ;
#5465 = CARTESIAN_POINT ( 'NONE',  ( 0.000000000000000000, 0.000000000000000000, 0.000000000000000000 ) ) ;
#5466 = AXIS2_PLACEMENT_3D ( 'NONE', #6811, #13296, #19752 ) ;
#5467 = VERTEX_POINT ( 'NONE', #3207 ) ;
#5468 = EDGE_CURVE ( 'NONE', #3247, #3717, #11704, .T. ) ;
#5469 = CARTESIAN_POINT ( 'NONE',  ( 30.87594499568497497, -110.8713507097124022, 79.29891132742112347 ) ) ;
#5470 = CARTESIAN_POINT ( 'NONE',  ( 6.358192988180014993, 4.248408729364578917, 18.34020625018030870 ) ) ;
#5471 = VERTEX_POINT ( 'NONE', #14141 ) ;
#5472 = CARTESIAN_POINT ( 'NONE',  ( 6.929096493489630859, -2.870125743571144472, 7.227762500180316074 ) ) ;
#5473 = CIRCLE ( 'NONE', #15989, 27.60000000002761311 ) ;
#5474 = ORIENTED_EDGE ( 'NONE', *, *, #9828, .F. ) ;
#5475 = DIRECTION ( 'NONE',  ( 0.000000000000000000, -0.6310879443260433153, -0.7757112907044274586 ) ) ;
#5476 = CARTESIAN_POINT ( 'NONE',  ( 6.888301784570727726, 16.62983158437509701, 0.7867625001803102425 ) ) ;
#5477 = EDGE_LOOP ( 'NONE', ( #19027, #19749, #1920, #8175 ) ) ;
#5478 = AXIS2_PLACEMENT_3D ( 'NONE', #19082, #4557, #4665 ) ;
#5479 = ORIENTED_EDGE ( 'NONE', *, *, #5963, .T. ) ;
#5480 = CARTESIAN_POINT ( 'NONE',  ( 0.000000000000000000, -64.79224928664393701, 2.456263514197400077 ) ) ;
#5481 = DIRECTION ( 'NONE',  ( -1.000000000000000000, 0.000000000000000000, -0.000000000000000000 ) ) ;
#5482 = CARTESIAN_POINT ( 'NONE',  ( 0.000000000000000000, 55.05624179291979914, 35.01774179823801347 ) ) ;
#5483 = FILL_AREA_STYLE ('',( #630 ) ) ;
#5484 = CARTESIAN_POINT ( 'NONE',  ( -2.870125741905213079, 6.929096494179683319, -15.15661249981968517 ) ) ;
#5485 = DIRECTION ( 'NONE',  ( -0.000000000000000000, -0.000000000000000000, 1.000000000000000000 ) ) ;
#5486 = CARTESIAN_POINT ( 'NONE',  ( 2.870125741905214412, -6.929096494179682431, 8.405887500180314831 ) ) ;
#5487 = CARTESIAN_POINT ( 'NONE',  ( 9.999999999999998224, 36.59093685910629290, 62.00889726308043493 ) ) ;
#5488 = AXIS2_PLACEMENT_3D ( 'NONE', #7460, #11082, #17121 ) ;
#5489 = CARTESIAN_POINT ( 'NONE',  ( 4.276731815070940357, 10.32494394706615815, -20.67229725028680676 ) ) ;
#5490 = VECTOR ( 'NONE', #16397, 1000.000000000000000 ) ;
#5491 = CYLINDRICAL_SURFACE ( 'NONE', #5648, 27.60000000002759535 ) ;
#5492 = ORIENTED_EDGE ( 'NONE', *, *, #12703, .F. ) ;
#5493 = FACE_OUTER_BOUND ( 'NONE', #15007, .T. ) ;
#5494 = CARTESIAN_POINT ( 'NONE',  ( 12.72792205982779734, -12.72792206288791128, 5.636675000180311201 ) ) ;
#5495 = DIRECTION ( 'NONE',  ( -1.000000000000000000, -0.000000000000000000, 0.000000000000000000 ) ) ;
#5496 = VECTOR ( 'NONE', #18616, 1000.000000000000000 ) ;
#5497 = EDGE_LOOP ( 'NONE', ( #12024, #148, #17837, #12677 ) ) ;
#5498 = DIRECTION ( 'NONE',  ( 0.000000000000000000, 0.000000000000000000, -1.000000000000000000 ) ) ;
#5499 = VERTEX_POINT ( 'NONE', #9676 ) ;
#5500 = CARTESIAN_POINT ( 'NONE',  ( 0.000000000000000000, -64.52323195238624010, -6.389157729493822657 ) ) ;
#5501 = DIRECTION ( 'NONE',  ( -1.000000000000000000, 0.000000000000000000, -0.000000000000000000 ) ) ;
#5502 = ORIENTED_EDGE ( 'NONE', *, *, #18042, .F. ) ;
#5503 = EDGE_LOOP ( 'NONE', ( #6884, #8768, #12320, #3041 ) ) ;
#5504 = CARTESIAN_POINT ( 'NONE',  ( 0.000000000000000000, 0.000000000000000000, 0.000000000000000000 ) ) ;
#5505 = VECTOR ( 'NONE', #9286, 1000.000000000000000 ) ;
#5506 = AXIS2_PLACEMENT_3D ( 'NONE', #18928, #20506, #3021 ) ;
#5507 = EDGE_CURVE ( 'NONE', #16541, #16592, #12657, .T. ) ;
#5508 = CARTESIAN_POINT ( 'NONE',  ( 17.00000000000000000, 2.516649172247811061E-16, -2.055000000000000160 ) ) ;
#5509 = DIRECTION ( 'NONE',  ( -1.000000000000000000, 0.000000000000000000, -0.000000000000000000 ) ) ;
#5510 = VECTOR ( 'NONE', #18888, 1000.000000000000114 ) ;
#5511 = CARTESIAN_POINT ( 'NONE',  ( -6.358192988180014993, -4.248408729364575365, -14.64729374981969023 ) ) ;
#5512 = CARTESIAN_POINT ( 'NONE',  ( 35.38680890825803971, -118.6613745440660921, -83.76770575229788562 ) ) ;
#5513 = DIRECTION ( 'NONE',  ( -0.000000000000000000, 0.000000000000000000, -1.000000000000000000 ) ) ;
#5514 = VECTOR ( 'NONE', #1660, 1000.000000000000000 ) ;
#5515 = CARTESIAN_POINT ( 'NONE',  ( 85.00002539999999840, 4.898587196589412829E-16, -4.000000000000000000 ) ) ;
#5516 = DIRECTION ( 'NONE',  ( -0.000000000000000000, -0.000000000000000000, 1.000000000000000000 ) ) ;
#5517 = AXIS2_PLACEMENT_3D ( 'NONE', #5090, #16027, #15916 ) ;
#5518 = VERTEX_POINT ( 'NONE', #6383 ) ;
#5519 = CARTESIAN_POINT ( 'NONE',  ( -1.491842754445842800, 7.500000000179346316, 3.987918750180313943 ) ) ;
#5520 = ORIENTED_EDGE ( 'NONE', *, *, #10415, .T. ) ;
#5521 = CARTESIAN_POINT ( 'NONE',  ( 16.62983158603122291, 6.888301780572502864, 11.38988750018031482 ) ) ;
#5522 = CARTESIAN_POINT ( 'NONE',  ( -12.15935632454279336, -17.74618724269112846, 72.30303056190481925 ) ) ;
#5523 = EDGE_LOOP ( 'NONE', ( #691, #1654, #8331, #14371 ) ) ;
#5524 = LINE ( 'NONE', #7221, #11941 ) ;
#5525 = VERTEX_POINT ( 'NONE', #16143 ) ;
#5526 = FACE_OUTER_BOUND ( 'NONE', #19612, .T. ) ;
#5527 = CARTESIAN_POINT ( 'NONE',  ( 19.99999999999999645, 0.000000000000000000, 0.000000000000000000 ) ) ;
#5528 = CIRCLE ( 'NONE', #15016, 72.00000000007199219 ) ;
#5529 = ORIENTED_EDGE ( 'NONE', *, *, #624, .F. ) ;
#5530 = CARTESIAN_POINT ( 'NONE',  ( 7.499999999820668783, -1.491842756249033508, -21.34176874981968908 ) ) ;
#5531 = CIRCLE ( 'NONE', #8934, 27.60000000002760601 ) ;
#5532 = EDGE_CURVE ( 'NONE', #14635, #16213, #14430, .T. ) ;
#5533 = LINE ( 'NONE', #578, #7024 ) ;
#5534 = CARTESIAN_POINT ( 'NONE',  ( 10.19618095047497697, -15.25966317163202923, -5.398393749819690335 ) ) ;
#5535 = AXIS2_PLACEMENT_3D ( 'NONE', #2899, #4486, #10848 ) ;
#5536 = CARTESIAN_POINT ( 'NONE',  ( -4.000000000000000000, 0.3904826640788061631, -5.600000000000000533 ) ) ;
#5537 = CIRCLE ( 'NONE', #10649, 4.250000000000000000 ) ;
#5538 = DIRECTION ( 'NONE',  ( 1.000000000000000000, 0.000000000000000000, 0.000000000000000000 ) ) ;
#5539 = CARTESIAN_POINT ( 'NONE',  ( 4.276731812588570492, -10.32494394809439697, 18.25979725064743064 ) ) ;
#5540 = EDGE_CURVE ( 'NONE', #15627, #11338, #2904, .T. ) ;
#5541 = ORIENTED_EDGE ( 'NONE', *, *, #15445, .F. ) ;
#5542 = CARTESIAN_POINT ( 'NONE',  ( -44.00000000000000000, -85.00000000000000000, 14.49999999999998579 ) ) ;
#5543 = DIRECTION ( 'NONE',  ( 1.000000000000000000, 0.000000000000000000, 0.000000000000000000 ) ) ;
#5544 = VERTEX_POINT ( 'NONE', #6279 ) ;
#5545 = CIRCLE ( 'NONE', #15717, 2.649999999999987477 ) ;
#5546 = CARTESIAN_POINT ( 'NONE',  ( 15.62350230547614416, -14.77425901644549278, -73.92464627053527693 ) ) ;
#5547 = ORIENTED_EDGE ( 'NONE', *, *, #16642, .F. ) ;
#5548 = CARTESIAN_POINT ( 'NONE',  ( 12.72792205982779734, -12.72792206288791128, 5.636675000180311201 ) ) ;
#5549 = FACE_OUTER_BOUND ( 'NONE', #7876, .T. ) ;
#5550 = LINE ( 'NONE', #2282, #1259 ) ;
#5551 = AXIS2_PLACEMENT_3D ( 'NONE', #36, #14866, #13073 ) ;
#5552 = ORIENTED_EDGE ( 'NONE', *, *, #10912, .F. ) ;
#5553 = LINE ( 'NONE', #8742, #10252 ) ;
#5554 = ORIENTED_EDGE ( 'NONE', *, *, #16443, .F. ) ;
#5555 = AXIS2_PLACEMENT_3D ( 'NONE', #17303, #15499, #7758 ) ;
#5556 = VERTEX_POINT ( 'NONE', #10947 ) ;
#5557 = DIRECTION ( 'NONE',  ( 0.000000000000000000, 0.8878852184023731109, 0.4600650377311559791 ) ) ;
#5558 = EDGE_LOOP ( 'NONE', ( #3066, #2977 ) ) ;
#5559 = DIRECTION ( 'NONE',  ( 0.000000000000000000, -1.224646799147341867E-16, 1.000000000000000000 ) ) ;
#5560 = CARTESIAN_POINT ( 'NONE',  ( 6.250000000000054179, 10.82531754730546147, 169.0000000000000000 ) ) ;
#5561 = CARTESIAN_POINT ( 'NONE',  ( 12.72792205982779912, -12.72792206288791483, -22.63832499981969448 ) ) ;
#5562 = CLOSED_SHELL ( 'NONE', ( #9857, #3415, #19859, #1195, #9801, #11703, #1979, #4251, #5743, #1423, #330, #11161, #20489, #10250, #1043, #18198, #7805, #6852, #9105, #18806, #10004, #13453, #2029, #16698, #11565, #15940, #19724, #10764, #19551, #13006, #17137, #7800, #14299, #16582, #4132, #8187, #7374 ) ) ;
#5563 = EDGE_CURVE ( 'NONE', #14001, #8060, #19119, .T. ) ;
#5564 = VERTEX_POINT ( 'NONE', #20484 ) ;
#5565 = EDGE_CURVE ( 'NONE', #788, #12290, #8307, .T. ) ;
#5566 = DIRECTION ( 'NONE',  ( 0.000000000000000000, 0.000000000000000000, -1.000000000000000000 ) ) ;
#5567 = CARTESIAN_POINT ( 'NONE',  ( -9.017423154539844887, -19.53047022166475699, 77.00824986274105299 ) ) ;
#5568 = CARTESIAN_POINT ( 'NONE',  ( 5.663308646854338768, -13.67243654778934747, -25.81060441848093134 ) ) ;
#5569 = CARTESIAN_POINT ( 'NONE',  ( 23.13963350654227824, -26.35784117651622793, -120.0000000000000142 ) ) ;
#5570 = ADVANCED_FACE ( 'NONE', ( #1532 ), #3100, .T. ) ;
#5571 = ORIENTED_EDGE ( 'NONE', *, *, #18940, .T. ) ;
#5572 = PRODUCT_RELATED_PRODUCT_CATEGORY ( 'part', '', ( #13215 ) ) ;
#5573 = ORIENTED_EDGE ( 'NONE', *, *, #7368, .T. ) ;
#5574 = CARTESIAN_POINT ( 'NONE',  ( 0.000000000000000000, 0.000000000000000000, 43.00000000000000000 ) ) ;
#5575 = FACE_OUTER_BOUND ( 'NONE', #11083, .T. ) ;
#5576 = VERTEX_POINT ( 'NONE', #7981 ) ;
#5577 = CARTESIAN_POINT ( 'NONE',  ( -1.485268882270375679, -22.96492952317579395, -75.38826545565814286 ) ) ;
#5578 = ORIENTED_EDGE ( 'NONE', *, *, #2115, .T. ) ;
#5579 = VECTOR ( 'NONE', #19315, 1000.000000000000000 ) ;
#5580 = DIRECTION ( 'NONE',  ( 1.000000000000000000, 0.000000000000000000, 0.000000000000000000 ) ) ;
#5581 = CARTESIAN_POINT ( 'NONE',  ( 16.62983158437509346, -6.888301784570737496, 12.56801250018031091 ) ) ;
#5582 = ORIENTED_EDGE ( 'NONE', *, *, #409, .F. ) ;
#5583 = ORIENTED_EDGE ( 'NONE', *, *, #10013, .F. ) ;
#5584 = CARTESIAN_POINT ( 'NONE',  ( 1.040949779275250179E-14, -85.00000000000000000, 5.000000000000000000 ) ) ;
#5585 = ADVANCED_FACE ( 'NONE', ( #14458, #9256, #15719, #6168 ), #14037, .F. ) ;
#5586 = DIRECTION ( 'NONE',  ( -1.000000000000000000, 0.000000000000000000, 0.000000000000000000 ) ) ;
#5587 = CARTESIAN_POINT ( 'NONE',  ( 19.99999999999999645, 31.17893654894229982, 57.31758819669181548 ) ) ;
#5588 = CARTESIAN_POINT ( 'NONE',  ( -15.25966316918061949, 10.19618095414378800, 19.47964375018031191 ) ) ;
#5589 = EDGE_CURVE ( 'NONE', #20286, #14728, #19823, .T. ) ;
#5590 = PRODUCT_DEFINITION_CONTEXT ( 'detailed design', #18739, 'design' ) ;
#5591 = VECTOR ( 'NONE', #17427, 1000.000000000000000 ) ;
#5592 = EDGE_CURVE ( 'NONE', #2692, #1099, #19493, .T. ) ;
#5593 = FILL_AREA_STYLE ('',( #7293 ) ) ;
#5594 = CARTESIAN_POINT ( 'NONE',  ( 5.303300858261588147, -5.303300859536636658, -1.608174999819685702 ) ) ;
#5595 = CARTESIAN_POINT ( 'NONE',  ( -6.358192988180021210, -4.248408729364580694, 19.89260625018031803 ) ) ;
#5596 = AXIS2_PLACEMENT_3D ( 'NONE', #1710, #11243, #9548 ) ;
#5597 = CARTESIAN_POINT ( 'NONE',  ( 9.474249098604504482, 6.330490856366291830, -10.36370350028680321 ) ) ;
#5598 = EDGE_CURVE ( 'NONE', #2326, #8735, #17831, .T. ) ;
#5599 = PRODUCT ( 'worm', 'worm', '', ( #12144 ) ) ;
#5600 = DIRECTION ( 'NONE',  ( 0.000000000000000000, 0.000000000000000000, 1.000000000000000000 ) ) ;
#5601 = ORIENTED_EDGE ( 'NONE', *, *, #649, .F. ) ;
#5602 = CARTESIAN_POINT ( 'NONE',  ( 19.99999999999999645, 0.000000000000000000, 0.000000000000000000 ) ) ;
#5603 = CARTESIAN_POINT ( 'NONE',  ( -15.25966317163203279, -10.19618095047498052, -10.56254374981969058 ) ) ;
#5604 = DIRECTION ( 'NONE',  ( 0.000000000000000000, 0.000000000000000000, 1.000000000000000000 ) ) ;
#5605 = ORIENTED_EDGE ( 'NONE', *, *, #9023, .T. ) ;
#5606 = CARTESIAN_POINT ( 'NONE',  ( -52.00000000000000000, -39.99999999999999289, 0.000000000000000000 ) ) ;
#5607 =( GEOMETRIC_REPRESENTATION_CONTEXT ( 3 ) GLOBAL_UNCERTAINTY_ASSIGNED_CONTEXT ( ( #13245 ) ) GLOBAL_UNIT_ASSIGNED_CONTEXT ( ( #16006, #17399, #206 ) ) REPRESENTATION_CONTEXT ( 'NONE', 'WORKASPACE' ) );
#5608 = ORIENTED_EDGE ( 'NONE', *, *, #15200, .F. ) ;
#5609 = CARTESIAN_POINT ( 'NONE',  ( 19.99999999999999645, 39.37110852956887186, -51.51683813304829584 ) ) ;
#5610 = CARTESIAN_POINT ( 'NONE',  ( 45.22159793441011999, -8.673994507468391291, -78.07221698934968401 ) ) ;
#5611 = AXIS2_PLACEMENT_3D ( 'NONE', #2439, #646, #2558 ) ;
#5612 = ORIENTED_EDGE ( 'NONE', *, *, #15320, .F. ) ;
#5613 = VERTEX_POINT ( 'NONE', #19218 ) ;
#5614 = DIRECTION ( 'NONE',  ( -1.000000000000000000, -0.000000000000000000, 0.000000000000000000 ) ) ;
#5615 = ADVANCED_FACE ( 'NONE', ( #4696 ), #11157, .T. ) ;
#5616 = AXIS2_PLACEMENT_3D ( 'NONE', #1013, #7457, #20176 ) ;
#5617 = AXIS2_PLACEMENT_3D ( 'NONE', #16739, #9088, #933 ) ;
#5618 = CYLINDRICAL_SURFACE ( 'NONE', #3158, 72.00000000007199219 ) ;
#5619 = AXIS2_PLACEMENT_3D ( 'NONE', #15087, #15284, #7224 ) ;
#5620 = CARTESIAN_POINT ( 'NONE',  ( 9.999999999999998224, -71.89099403602357086, 3.960426305688546922 ) ) ;
#5621 = AXIS2_PLACEMENT_3D ( 'NONE', #7662, #20592, #6067 ) ;
#5622 = CARTESIAN_POINT ( 'NONE',  ( -5.303300859536631329, -5.303300858261583706, -5.516824999819688990 ) ) ;
#5623 = CARTESIAN_POINT ( 'NONE',  ( 0.000000000000000000, 20.34307325858786442, 69.06634035770315450 ) ) ;
#5624 = CYLINDRICAL_SURFACE ( 'NONE', #680, 7.500000000000000000 ) ;
#5625 = DIRECTION ( 'NONE',  ( 0.000000000000000000, 0.5000000000000012212, 0.8660254037844380415 ) ) ;
#5626 = DIRECTION ( 'NONE',  ( 1.000000000000000000, 0.000000000000000000, 0.000000000000000000 ) ) ;
#5627 = AXIS2_PLACEMENT_3D ( 'NONE', #16922, #10149, #10466 ) ;
#5628 = VECTOR ( 'NONE', #8952, 1000.000000000000000 ) ;
#5629 = EDGE_LOOP ( 'NONE', ( #18866, #81, #10256, #5608 ) ) ;
#5630 = EDGE_CURVE ( 'NONE', #6239, #15053, #19415, .T. ) ;
#5631 =( GEOMETRIC_REPRESENTATION_CONTEXT ( 3 ) GLOBAL_UNCERTAINTY_ASSIGNED_CONTEXT ( ( #19802 ) ) GLOBAL_UNIT_ASSIGNED_CONTEXT ( ( #20023, #12192, #9229 ) ) REPRESENTATION_CONTEXT ( 'NONE', 'WORKASPACE' ) );
#5632 = CARTESIAN_POINT ( 'NONE',  ( -7.500000000000009770, 9.706494107251932559E-15, 1.926200000002316060 ) ) ;
#5633 = EDGE_LOOP ( 'NONE', ( #1364, #18096, #13595, #18836 ) ) ;
#5634 = CARTESIAN_POINT ( 'NONE',  ( 15.25966316918061416, -10.19618095414378622, 3.437543750180314994 ) ) ;
#5635 = CARTESIAN_POINT ( 'NONE',  ( -20.48001470518130418, -6.654962914332833712, 79.70582905289666087 ) ) ;
#5636 = ORIENTED_EDGE ( 'NONE', *, *, #4933, .T. ) ;
#5637 = LINE ( 'NONE', #16883, #12650 ) ;
#5638 = ORIENTED_EDGE ( 'NONE', *, *, #11033, .F. ) ;
#5639 = CARTESIAN_POINT ( 'NONE',  ( 17.50000000000000355, 0.000000000000000000, 126.0000000000000000 ) ) ;
#5640 = FACE_OUTER_BOUND ( 'NONE', #14676, .T. ) ;
#5641 = AXIS2_PLACEMENT_3D ( 'NONE', #14213, #10916, #15894 ) ;
#5642 = ORIENTED_EDGE ( 'NONE', *, *, #12153, .F. ) ;
#5643 = CARTESIAN_POINT ( 'NONE',  ( 0.000000000000000000, 44.69367065308723141, -56.44887778834702630 ) ) ;
#5644 = AXIS2_PLACEMENT_3D ( 'NONE', #19883, #18290, #2391 ) ;
#5645 = CARTESIAN_POINT ( 'NONE',  ( 0.000000000000000000, 10.77748419466696284, 63.93680186330476545 ) ) ;
#5646 = CARTESIAN_POINT ( 'NONE',  ( 10.19618095414378622, 15.25966316918061239, -17.76870624981969371 ) ) ;
#5647 = LINE ( 'NONE', #12123, #6896 ) ;
#5648 = AXIS2_PLACEMENT_3D ( 'NONE', #18550, #10383, #5600 ) ;
#5649 = DIRECTION ( 'NONE',  ( 0.000000000000000000, -0.9976687691905398170, 0.06824241336466078944 ) ) ;
#5650 = CARTESIAN_POINT ( 'NONE',  ( 9.474249098604511587, 6.330490856366296271, -3.240983999352573086 ) ) ;
#5651 = ORIENTED_EDGE ( 'NONE', *, *, #17762, .T. ) ;
#5652 =( NAMED_UNIT ( * ) PLANE_ANGLE_UNIT ( ) SI_UNIT ( $, .RADIAN. ) );
#5653 = CARTESIAN_POINT ( 'NONE',  ( -10.00000000000000000, 0.000000000000000000, 0.000000000000000000 ) ) ;
#5654 = ORIENTED_EDGE ( 'NONE', *, *, #3124, .T. ) ;
#5655 = AXIS2_PLACEMENT_3D ( 'NONE', #4118, #967, #9216 ) ;
#5656 = CARTESIAN_POINT ( 'NONE',  ( -12.15935632454278625, -17.74618724269114622, -72.30303056190483346 ) ) ;
#5657 = EDGE_LOOP ( 'NONE', ( #20578, #2412, #16192, #17829 ) ) ;
#5658 = EDGE_CURVE ( 'NONE', #231, #5157, #12961, .T. ) ;
#5659 = CIRCLE ( 'NONE', #1287, 27.60000000002760245 ) ;
#5660 = CARTESIAN_POINT ( 'NONE',  ( 6.888301784570728614, 16.62983158437510056, 2.691362500180312978 ) ) ;
#5661 = CARTESIAN_POINT ( 'NONE',  ( 0.000000000000000000, 49.77519642624066165, -42.18840861821735189 ) ) ;
#5662 = DIRECTION ( 'NONE',  ( -1.000000000000000000, -0.000000000000000000, -0.000000000000000000 ) ) ;
#5663 = ORIENTED_EDGE ( 'NONE', *, *, #11143, .T. ) ;
#5664 = CIRCLE ( 'NONE', #16837, 27.60000000002759890 ) ;
#5665 = DIRECTION ( 'NONE',  ( 0.000000000000000000, 0.000000000000000000, -1.000000000000000000 ) ) ;
#5666 = EDGE_LOOP ( 'NONE', ( #2723, #15129, #3200, #14766, #3981, #15027, #19429 ) ) ;
#5667 = CARTESIAN_POINT ( 'NONE',  ( 6.358192988180019434, 4.248408729364581582, 15.18010625018031590 ) ) ;
#5668 = ORIENTED_EDGE ( 'NONE', *, *, #3531, .T. ) ;
#5669 = FACE_OUTER_BOUND ( 'NONE', #8609, .T. ) ;
#5670 = DIRECTION ( 'NONE',  ( -1.000000000000000000, -0.000000000000000000, -0.000000000000000000 ) ) ;
#5671 = AXIS2_PLACEMENT_3D ( 'NONE', #3475, #11451, #6559 ) ;
#5672 = CARTESIAN_POINT ( 'NONE',  ( -62.49999999999999289, -40.00000000000000000, 5.000000000000000000 ) ) ;
#5673 = CONTEXT_DEPENDENT_SHAPE_REPRESENTATION ( #8443, #11694 ) ;
#5674 = CARTESIAN_POINT ( 'NONE',  ( 10.46442989202484064, -10.46442989454075878, -1.931583081158455562 ) ) ;
#5675 = ORIENTED_EDGE ( 'NONE', *, *, #13509, .F. ) ;
#5676 = CARTESIAN_POINT ( 'NONE',  ( 0.000000000000000000, -56.42118728228132341, -32.77318456705499017 ) ) ;
#5677 = VERTEX_POINT ( 'NONE', #14557 ) ;
#5678 = CARTESIAN_POINT ( 'NONE',  ( -18.23093333169988739, -11.40057928256656439, 82.28885341040493984 ) ) ;
#5679 = CARTESIAN_POINT ( 'NONE',  ( 5.663308646854338768, -13.67243654778934747, -16.38560441848093063 ) ) ;
#5680 = DIRECTION ( 'NONE',  ( -1.000000000000000000, -0.000000000000000000, 0.000000000000000000 ) ) ;
#5681 = ORIENTED_EDGE ( 'NONE', *, *, #13908, .T. ) ;
#5682 = DIRECTION ( 'NONE',  ( 0.000000000000000000, -0.3984010898462296835, -0.9172113015054581542 ) ) ;
#5683 = DIRECTION ( 'NONE',  ( 0.000000000000000000, 0.000000000000000000, 1.000000000000000000 ) ) ;
#5684 = VERTEX_POINT ( 'NONE', #5007 ) ;
#5685 = EDGE_CURVE ( 'NONE', #12949, #13448, #8667, .T. ) ;
#5686 = DIRECTION ( 'NONE',  ( 0.000000000000000000, 0.000000000000000000, 1.000000000000000000 ) ) ;
#5687 = VERTEX_POINT ( 'NONE', #6786 ) ;
#5688 = DIRECTION ( 'NONE',  ( 0.000000000000000000, -0.1361666490962331333, -0.9906859460363326431 ) ) ;
#5689 = CARTESIAN_POINT ( 'NONE',  ( -3.580422614997674557, -17.99999999956957808, 5.204731250180310909 ) ) ;
#5690 = EDGE_CURVE ( 'NONE', #12410, #18310, #16782, .T. ) ;
#5691 = ORIENTED_EDGE ( 'NONE', *, *, #10428, .F. ) ;
#5692 = ORIENTED_EDGE ( 'NONE', *, *, #7126, .T. ) ;
#5693 = CARTESIAN_POINT ( 'NONE',  ( 45.22159793441013420, -8.673994507468389514, -84.62946326583126222 ) ) ;
#5694 = DIRECTION ( 'NONE',  ( -0.8191520442889896891, 0.000000000000000000, -0.5735764363510490460 ) ) ;
#5695 = FACE_OUTER_BOUND ( 'NONE', #18, .T. ) ;
#5696 = CARTESIAN_POINT ( 'NONE',  ( -10.00000000000000000, 0.000000000000000000, 0.000000000000000000 ) ) ;
#5697 = ADVANCED_FACE ( 'NONE', ( #16241 ), #14753, .T. ) ;
#5698 = CARTESIAN_POINT ( 'NONE',  ( -12.72792206288791483, -12.72792205982780089, 17.41792500018031120 ) ) ;
#5699 = DIRECTION ( 'NONE',  ( 1.000000000000000000, 0.000000000000000000, 0.000000000000000000 ) ) ;
#5700 = CARTESIAN_POINT ( 'NONE',  ( 9.015937996181842420E-10, 7.500000000000007994, 4.282450000180314298 ) ) ;
#5701 = DIRECTION ( 'NONE',  ( -0.000000000000000000, -0.000000000000000000, 1.000000000000000000 ) ) ;
#5702 = CARTESIAN_POINT ( 'NONE',  ( 6.330490856366289165, -9.474249098604506258, -17.43245350028680107 ) ) ;
#5703 = DIRECTION ( 'NONE',  ( -1.000000000000000000, -0.000000000000000000, -0.000000000000000000 ) ) ;
#5704 = EDGE_CURVE ( 'NONE', #20245, #12949, #6475, .T. ) ;
#5705 = VERTEX_POINT ( 'NONE', #3315 ) ;
#5706 = CARTESIAN_POINT ( 'NONE',  ( 0.000000000000000000, 0.000000000000000000, 0.000000000000000000 ) ) ;
#5707 = CARTESIAN_POINT ( 'NONE',  ( -18.00000000043041126, -3.580422610670022543, -0.5484812498196892649 ) ) ;
#5708 = CARTESIAN_POINT ( 'NONE',  ( -12.50000000000000533, 0.000000000000000000, 46.00000000000000711 ) ) ;
#5709 = VERTEX_POINT ( 'NONE', #18243 ) ;
#5710 = ADVANCED_FACE ( 'NONE', ( #6894 ), #19721, .T. ) ;
#5711 = CARTESIAN_POINT ( 'NONE',  ( -24.99999999999999289, -85.00000000000000000, 74.99999999999998579 ) ) ;
#5712 = ORIENTED_EDGE ( 'NONE', *, *, #20634, .F. ) ;
#5713 = CARTESIAN_POINT ( 'NONE',  ( 0.000000000000000000, 70.68211945903209426, -13.71269443944134458 ) ) ;
#5714 = CARTESIAN_POINT ( 'NONE',  ( 36.29350642860042342, -22.37888450698892484, -70.21894222985346801 ) ) ;
#5715 = EDGE_CURVE ( 'NONE', #964, #12005, #14092, .T. ) ;
#5716 = ORIENTED_EDGE ( 'NONE', *, *, #14562, .T. ) ;
#5717 = VERTEX_POINT ( 'NONE', #5204 ) ;
#5718 = DIRECTION ( 'NONE',  ( 0.000000000000000000, 0.000000000000000000, 1.000000000000000000 ) ) ;
#5719 = ADVANCED_FACE ( 'NONE', ( #18035 ), #3708, .T. ) ;
#5720 = FILL_AREA_STYLE_COLOUR ( '', #11738 ) ;
#5721 = DIRECTION ( 'NONE',  ( 1.000000000000000000, 0.000000000000000000, -0.000000000000000000 ) ) ;
#5722 = CARTESIAN_POINT ( 'NONE',  ( 19.99999999999999645, 28.84646472442454979, 58.52617768068444093 ) ) ;
#5723 = CARTESIAN_POINT ( 'NONE',  ( 5.303300859536630441, 5.303300858261584594, -0.8043249998196875250 ) ) ;
#5724 = DIRECTION ( 'NONE',  ( 0.000000000000000000, 0.000000000000000000, 1.000000000000000000 ) ) ;
#5725 = FACE_OUTER_BOUND ( 'NONE', #6417, .T. ) ;
#5726 = ADVANCED_FACE ( 'NONE', ( #10183 ), #9870, .T. ) ;
#5727 = CARTESIAN_POINT ( 'NONE',  ( 21.00000000000000355, 0.000000000000000000, 2.055000000000000160 ) ) ;
#5728 = DIRECTION ( 'NONE',  ( -1.000000000000000000, -0.000000000000000000, -0.000000000000000000 ) ) ;
#5729 = EDGE_CURVE ( 'NONE', #10676, #2005, #892, .T. ) ;
#5730 = CIRCLE ( 'NONE', #13536, 27.60000000002759890 ) ;
#5731 = EDGE_CURVE ( 'NONE', #7518, #13187, #12050, .T. ) ;
#5732 = ORIENTED_EDGE ( 'NONE', *, *, #18089, .T. ) ;
#5733 = DIRECTION ( 'NONE',  ( 0.000000000000000000, 0.000000000000000000, 1.000000000000000000 ) ) ;
#5734 = EDGE_LOOP ( 'NONE', ( #15280, #17496, #14310 ) ) ;
#5735 = CARTESIAN_POINT ( 'NONE',  ( -18.00000000043041126, -3.580422610670022543, -2.453081249819689003 ) ) ;
#5736 = CARTESIAN_POINT ( 'NONE',  ( 14.60954982181483963, -15.77788197283120120, 73.35099031848520212 ) ) ;
#5737 = ORIENTED_EDGE ( 'NONE', *, *, #19216, .F. ) ;
#5738 = DIRECTION ( 'NONE',  ( 0.000000000000000000, 0.000000000000000000, 1.000000000000000000 ) ) ;
#5739 = ORIENTED_EDGE ( 'NONE', *, *, #12695, .F. ) ;
#5740 = DIRECTION ( 'NONE',  ( -1.000000000000000000, 0.000000000000000000, 0.000000000000000000 ) ) ;
#5741 = DIRECTION ( 'NONE',  ( -1.000000000000000000, -0.000000000000000000, -0.000000000000000000 ) ) ;
#5742 = CARTESIAN_POINT ( 'NONE',  ( 19.99999999999999645, 0.000000000000000000, 0.000000000000000000 ) ) ;
#5743 = ADVANCED_FACE ( 'NONE', ( #16336 ), #8088, .T. ) ;
#5744 = ORIENTED_EDGE ( 'NONE', *, *, #5844, .T. ) ;
#5745 = FACE_OUTER_BOUND ( 'NONE', #8298, .T. ) ;
#5746 = DIRECTION ( 'NONE',  ( -1.000000000000000000, -0.000000000000000000, 0.000000000000000000 ) ) ;
#5747 = CARTESIAN_POINT ( 'NONE',  ( 2.163825119083639120E-09, 17.99999999999999645, -18.65229999981968945 ) ) ;
#5748 = DIRECTION ( 'NONE',  ( 1.000000000000000000, 0.000000000000000000, 0.000000000000000000 ) ) ;
#5749 = DIRECTION ( 'NONE',  ( 0.000000000000000000, 0.5195839500354287877, 0.8544194045464914566 ) ) ;
#5750 = CARTESIAN_POINT ( 'NONE',  ( 2.222972768810839383, -11.17563879758428769, -9.720671499352569356 ) ) ;
#5751 = ORIENTED_EDGE ( 'NONE', *, *, #14798, .T. ) ;
#5752 = CARTESIAN_POINT ( 'NONE',  ( 19.99999999999999645, 0.9548212943365497196, 71.99366858485716136 ) ) ;
#5753 = CYLINDRICAL_SURFACE ( 'NONE', #18979, 17.50000000000000355 ) ;
#5754 = AXIS2_PLACEMENT_3D ( 'NONE', #9894, #8200, #353 ) ;
#5755 = VERTEX_POINT ( 'NONE', #8480 ) ;
#5756 = CARTESIAN_POINT ( 'NONE',  ( 17.61872475889259704, -12.39310755016574817, -75.38263485905285677 ) ) ;
#5757 = EDGE_LOOP ( 'NONE', ( #12689, #1251, #6437, #10079 ) ) ;
#5758 = CARTESIAN_POINT ( 'NONE',  ( -3.580422610670018546, 18.00000000043041126, -7.617231249819687910 ) ) ;
#5759 = FACE_OUTER_BOUND ( 'NONE', #7158, .T. ) ;
#5760 = FACE_OUTER_BOUND ( 'NONE', #14979, .T. ) ;
#5761 = VERTEX_POINT ( 'NONE', #5096 ) ;
#5762 = CARTESIAN_POINT ( 'NONE',  ( -24.99999999999999645, -85.00000000000000000, -1.040949779275250179E-14 ) ) ;
#5763 = EDGE_LOOP ( 'NONE', ( #7249, #17695, #4364, #1441 ) ) ;
#5764 = LINE ( 'NONE', #13945, #10221 ) ;
#5765 = AXIS2_PLACEMENT_3D ( 'NONE', #19531, #1734, #4908 ) ;
#5766 = ORIENTED_EDGE ( 'NONE', *, *, #7546, .T. ) ;
#5767 = VECTOR ( 'NONE', #18249, 1000.000000000000000 ) ;
#5768 = VECTOR ( 'NONE', #4897, 1000.000000000000000 ) ;
#5769 = CARTESIAN_POINT ( 'NONE',  ( -4.000000000000000000, 2.309401076758531346, -5.242734410091827613 ) ) ;
#5770 = EDGE_CURVE ( 'NONE', #65, #12993, #11564, .T. ) ;
#5771 = PRODUCT_DEFINITION_SHAPE ( 'NONE', 'NONE',  #17130 ) ;
#5772 = EDGE_CURVE ( 'NONE', #18485, #13263, #8385, .T. ) ;
#5773 = CARTESIAN_POINT ( 'NONE',  ( 8.899999999999895550, -10.82531754730554496, 46.00000000000000711 ) ) ;
#5774 = CONTEXT_DEPENDENT_SHAPE_REPRESENTATION ( #18209, #16943 ) ;
#5775 = CARTESIAN_POINT ( 'NONE',  ( 13.67243654778935991, 5.663308646854338768, 5.726229418841543684 ) ) ;
#5776 = ORIENTED_EDGE ( 'NONE', *, *, #9616, .F. ) ;
#5777 = FACE_OUTER_BOUND ( 'NONE', #14057, .T. ) ;
#5778 = ORIENTED_EDGE ( 'NONE', *, *, #15573, .T. ) ;
#5779 = CARTESIAN_POINT ( 'NONE',  ( -20.81434048145373339, -5.479059011584746841, 87.82828572917365761 ) ) ;
#5780 = CARTESIAN_POINT ( 'NONE',  ( -15.25966317163202923, -10.19618095047497874, 6.382856250180309665 ) ) ;
#5781 = CARTESIAN_POINT ( 'NONE',  ( -7.500000000000000888, 1.491842755816075172, -22.89416874991221462 ) ) ;
#5782 = VECTOR ( 'NONE', #17182, 1000.000000000000114 ) ;
#5783 = DIRECTION ( 'NONE',  ( -1.000000000000000000, 0.000000000000000000, -0.000000000000000000 ) ) ;
#5784 = ORIENTED_EDGE ( 'NONE', *, *, #14654, .F. ) ;
#5785 = CARTESIAN_POINT ( 'NONE',  ( 52.00000000000000000, -99.99999999999998579, 0.000000000000000000 ) ) ;
#5786 = CARTESIAN_POINT ( 'NONE',  ( 19.99999999999999645, 0.000000000000000000, 0.000000000000000000 ) ) ;
#5787 = VECTOR ( 'NONE', #7320, 1000.000000000000000 ) ;
#5788 = ORIENTED_EDGE ( 'NONE', *, *, #13299, .T. ) ;
#5789 = CARTESIAN_POINT ( 'NONE',  ( 30.00000000000000000, -122.0000000000000000, -2.099999999999997424 ) ) ;
#5790 = EDGE_LOOP ( 'NONE', ( #2125, #17938, #8399, #2575 ) ) ;
#5791 = LINE ( 'NONE', #2637, #12935 ) ;
#5792 = CARTESIAN_POINT ( 'NONE',  ( -10.19618095414378445, -15.25966316918061239, -13.05620624981969335 ) ) ;
#5793 = VERTEX_POINT ( 'NONE', #5404 ) ;
#5794 = ORIENTED_EDGE ( 'NONE', *, *, #9338, .F. ) ;
#5795 = DIRECTION ( 'NONE',  ( 0.000000000000000000, 0.9790840876823234673, -0.2034560130526309185 ) ) ;
#5796 = AXIS2_PLACEMENT_3D ( 'NONE', #14734, #16011, #211 ) ;
#5797 = VECTOR ( 'NONE', #8019, 1000.000000000000000 ) ;
#5798 = DIRECTION ( 'NONE',  ( 0.000000000000000000, 0.000000000000000000, -1.000000000000000000 ) ) ;
#5799 = EDGE_CURVE ( 'NONE', #3107, #6625, #4939, .T. ) ;
#5800 = CYLINDRICAL_SURFACE ( 'NONE', #13436, 7.500000000000000000 ) ;
#5801 = DIRECTION ( 'NONE',  ( 1.000000000000000000, 0.000000000000000000, 0.000000000000000000 ) ) ;
#5802 = VECTOR ( 'NONE', #9942, 1000.000000000000000 ) ;
#5803 = CARTESIAN_POINT ( 'NONE',  ( -3.580422610670018990, 18.00000000043041481, 1.807768750180308137 ) ) ;
#5804 = UNCERTAINTY_MEASURE_WITH_UNIT (LENGTH_MEASURE( 1.000000000000000082E-05 ), #19495, 'distance_accuracy_value', 'NONE');
#5805 = CARTESIAN_POINT ( 'NONE',  ( -6.358192988180021210, -4.248408729364580694, -17.80739374981969192 ) ) ;
#5806 = ORIENTED_EDGE ( 'NONE', *, *, #10782, .T. ) ;
#5807 = CIRCLE ( 'NONE', #17675, 2.649999999999998579 ) ;
#5808 = CARTESIAN_POINT ( 'NONE',  ( 2.500000000000000000, 1.178949249685212974, -2.042000000000001148 ) ) ;
#5809 = EDGE_CURVE ( 'NONE', #2556, #14202, #13482, .T. ) ;
#5810 = CARTESIAN_POINT ( 'NONE',  ( -14.79893867722910095, 2.943691928843434891, 15.12923933151907718 ) ) ;
#5811 = CARTESIAN_POINT ( 'NONE',  ( 11.50000000000000000, 0.000000000000000000, 81.99999999999998579 ) ) ;
#5812 = AXIS2_PLACEMENT_3D ( 'NONE', #3210, #18222, #6384 ) ;
#5813 = AXIS2_PLACEMENT_3D ( 'NONE', #15275, #2038, #459 ) ;
#5814 = VERTEX_POINT ( 'NONE', #19925 ) ;
#5815 = CARTESIAN_POINT ( 'NONE',  ( 40.00000000000000711, 39.99999999999998579, -130.0000000000000000 ) ) ;
#5816 = CARTESIAN_POINT ( 'NONE',  ( -10.19618095414378622, -15.25966316918061416, -20.57660624981969377 ) ) ;
#5817 = CARTESIAN_POINT ( 'NONE',  ( -27.96694501150314593, -24.74873734152930993, -120.0000000000000142 ) ) ;
#5818 = AXIS2_PLACEMENT_3D ( 'NONE', #20454, #2661, #4121 ) ;
#5819 = ORIENTED_EDGE ( 'NONE', *, *, #12489, .T. ) ;
#5820 = EDGE_CURVE ( 'NONE', #18485, #7631, #6622, .T. ) ;
#5821 = CARTESIAN_POINT ( 'NONE',  ( 5.200000000000002842, 0.000000000000000000, 0.000000000000000000 ) ) ;
#5822 = ORIENTED_EDGE ( 'NONE', *, *, #12206, .T. ) ;
#5823 = CARTESIAN_POINT ( 'NONE',  ( 0.000000000000000000, 0.000000000000000000, 0.000000000000000000 ) ) ;
#5824 = CARTESIAN_POINT ( 'NONE',  ( -12.50000000000000533, 0.000000000000000000, 43.00000000000000000 ) ) ;
#5825 = ORIENTED_EDGE ( 'NONE', *, *, #11135, .T. ) ;
#5826 = EDGE_LOOP ( 'NONE', ( #5554, #4382 ) ) ;
#5827 = CARTESIAN_POINT ( 'NONE',  ( 0.000000000000000000, -64.79224928664389438, -2.456263514198281150 ) ) ;
#5828 = CYLINDRICAL_SURFACE ( 'NONE', #7556, 65.24900000006525147 ) ;
#5829 = CIRCLE ( 'NONE', #15652, 27.60000000002760245 ) ;
#5830 = AXIS2_PLACEMENT_3D ( 'NONE', #4345, #738, #7623 ) ;
#5831 = CLOSED_SHELL ( 'NONE', ( #7561, #4377, #3150, #11560, #10615, #16078, #16476, #14622, #3641, #20916, #17510, #15172, #9128, #9125, #9488, #8529, #7953, #19336, #18369, #18454, #6623, #19843, #8417, #14405, #20571, #12592, #4166 ) ) ;
#5832 = CARTESIAN_POINT ( 'NONE',  ( 0.000000000000000000, 0.000000000000000000, -130.0000000000000000 ) ) ;
#5833 = AXIS2_PLACEMENT_3D ( 'NONE', #3752, #19660, #16495 ) ;
#5834 = EDGE_CURVE ( 'NONE', #14416, #14958, #20162, .T. ) ;
#5835 = CARTESIAN_POINT ( 'NONE',  ( 5.303300859536630441, 5.303300858261584594, -10.22932499981969023 ) ) ;
#5836 = EDGE_CURVE ( 'NONE', #11468, #17275, #14444, .T. ) ;
#5837 =( LENGTH_UNIT ( ) NAMED_UNIT ( * ) SI_UNIT ( .MILLI., .METRE. ) );
#5838 = CIRCLE ( 'NONE', #13982, 27.60000000002759890 ) ;
#5839 = CARTESIAN_POINT ( 'NONE',  ( 19.99999999999999645, 27.62776854598936538, -58.65812137498974721 ) ) ;
#5840 = CARTESIAN_POINT ( 'NONE',  ( 9.999999999999998224, 71.89099403602354244, -3.960426305689050075 ) ) ;
#5841 = VERTEX_POINT ( 'NONE', #3809 ) ;
#5842 = DIRECTION ( 'NONE',  ( -1.000000000000000000, -0.000000000000000000, -0.000000000000000000 ) ) ;
#5843 = ORIENTED_EDGE ( 'NONE', *, *, #4093, .T. ) ;
#5844 = EDGE_CURVE ( 'NONE', #2530, #16859, #18482, .T. ) ;
#5845 = CARTESIAN_POINT ( 'NONE',  ( 16.62983158437509346, -6.888301784570739272, 3.143012500180314639 ) ) ;
#5846 = CARTESIAN_POINT ( 'NONE',  ( -15.14999999999999325, 0.000000000000000000, 166.0000000000000000 ) ) ;
#5847 = EDGE_CURVE ( 'NONE', #5038, #17353, #204, .T. ) ;
#5848 = CIRCLE ( 'NONE', #15668, 27.60000000002759890 ) ;
#5849 = ORIENTED_EDGE ( 'NONE', *, *, #17993, .F. ) ;
#5850 = VECTOR ( 'NONE', #2702, 1000.000000000000000 ) ;
#5851 = DIRECTION ( 'NONE',  ( 0.000000000000000000, 0.000000000000000000, -1.000000000000000000 ) ) ;
#5852 = EDGE_LOOP ( 'NONE', ( #8337, #9933, #12486, #2037 ) ) ;
#5853 = CARTESIAN_POINT ( 'NONE',  ( 43.74543371413037107, -125.0989072405818661, 82.69023214352036177 ) ) ;
#5854 = DIRECTION ( 'NONE',  ( -1.000000000000000000, -0.000000000000000000, 0.000000000000000000 ) ) ;
#5855 = LINE ( 'NONE', #20265, #1301 ) ;
#5856 =( GEOMETRIC_REPRESENTATION_CONTEXT ( 3 ) GLOBAL_UNCERTAINTY_ASSIGNED_CONTEXT ( ( #2420 ) ) GLOBAL_UNIT_ASSIGNED_CONTEXT ( ( #14805, #5140, #3552 ) ) REPRESENTATION_CONTEXT ( 'NONE', 'WORKASPACE' ) );
#5857 = ORIENTED_EDGE ( 'NONE', *, *, #9463, .F. ) ;
#5858 = CARTESIAN_POINT ( 'NONE',  ( 19.99999999999999645, -46.01927912072559224, 45.67597560296373871 ) ) ;
#5859 = ADVANCED_FACE ( 'NONE', ( #16755 ), #7200, .T. ) ;
#5860 = AXIS2_PLACEMENT_3D ( 'NONE', #10962, #4285, #19018 ) ;
#5861 = CARTESIAN_POINT ( 'NONE',  ( 46.54332301554113371, -6.983203288388278196, 86.24273042526077404 ) ) ;
#5862 = CARTESIAN_POINT ( 'NONE',  ( 7.500000000000004441, -8.788009017158368372E-15, -9.051199999997692203 ) ) ;
#5863 = CARTESIAN_POINT ( 'NONE',  ( -12.50000000000000533, 0.000000000000000000, 46.00000000000000711 ) ) ;
#5864 = AXIS2_PLACEMENT_3D ( 'NONE', #18345, #16959, #3921 ) ;
#5865 = EDGE_CURVE ( 'NONE', #5564, #15624, #8004, .T. ) ;
#5866 = DIRECTION ( 'NONE',  ( 0.000000000000000000, 0.000000000000000000, 1.000000000000000000 ) ) ;
#5867 = AXIS2_PLACEMENT_3D ( 'NONE', #20163, #2589, #10213 ) ;
#5869 = VERTEX_POINT ( 'NONE', #6998 ) ;
#5868 = VECTOR ( 'NONE', #20149, 1000.000000000000000 ) ;
#5870 = FACE_OUTER_BOUND ( 'NONE', #10343, .T. ) ;
#5871 = EDGE_CURVE ( 'NONE', #18341, #1116, #3261, .T. ) ;
#5872 = CARTESIAN_POINT ( 'NONE',  ( -31.74999999999995737, 3.061616997868383634E-16, -2.500000000000000444 ) ) ;
#5873 = ORIENTED_EDGE ( 'NONE', *, *, #10339, .T. ) ;
#5874 = CARTESIAN_POINT ( 'NONE',  ( 19.99999999999999645, 38.69327817041845918, -52.53819777490596010 ) ) ;
#5875 = CARTESIAN_POINT ( 'NONE',  ( 0.000000000000000000, -59.36728637278046961, 40.73727173906768684 ) ) ;
#5876 = ADVANCED_FACE ( 'NONE', ( #20022 ), #3917, .T. ) ;
#5877 = EDGE_LOOP ( 'NONE', ( #9809, #584, #17386, #4043 ) ) ;
#5878 = CARTESIAN_POINT ( 'NONE',  ( 18.00000000000000000, -2.163824016901520184E-09, -14.39144999981968986 ) ) ;
#5879 = CARTESIAN_POINT ( 'NONE',  ( 50.00000000000000000, -159.9999999999999716, 85.00000000000000000 ) ) ;
#5880 = CARTESIAN_POINT ( 'NONE',  ( -14.49999999999998934, -85.00000000000000000, 19.00000000000000000 ) ) ;
#5881 = AXIS2_PLACEMENT_3D ( 'NONE', #13178, #9785, #37 ) ;
#5882 = ORIENTED_EDGE ( 'NONE', *, *, #9510, .F. ) ;
#5883 = VECTOR ( 'NONE', #19979, 1000.000000000000000 ) ;
#5884 = VECTOR ( 'NONE', #3109, 1000.000000000000000 ) ;
#5885 = CARTESIAN_POINT ( 'NONE',  ( 7.500000000000000000, 9.184850993605147944E-16, 40.00000000000000000 ) ) ;
#5886 = ORIENTED_EDGE ( 'NONE', *, *, #8367, .T. ) ;
#5887 = DIRECTION ( 'NONE',  ( -1.000000000000000000, -0.000000000000000000, -0.000000000000000000 ) ) ;
#5888 = EDGE_LOOP ( 'NONE', ( #7301, #10862, #14835, #19480 ) ) ;
#5889 = CIRCLE ( 'NONE', #17742, 10.00000000000000178 ) ;
#5890 = AXIS2_PLACEMENT_3D ( 'NONE', #7652, #20365, #14133 ) ;
#5891 = CIRCLE ( 'NONE', #1517, 72.00000000007199219 ) ;
#5892 = DIRECTION ( 'NONE',  ( 0.000000000000000000, 0.000000000000000000, 1.000000000000000000 ) ) ;
#5893 = EDGE_CURVE ( 'NONE', #18535, #17067, #5968, .T. ) ;
#5894 = DIRECTION ( 'NONE',  ( 0.000000000000000000, 0.000000000000000000, 1.000000000000000000 ) ) ;
#5895 = CARTESIAN_POINT ( 'NONE',  ( 12.54593441562640876, -8.382925371439629458, 7.198885668841548124 ) ) ;
#5896 = ORIENTED_EDGE ( 'NONE', *, *, #4654, .F. ) ;
#5897 = CARTESIAN_POINT ( 'NONE',  ( -10.00000000000000000, 0.000000000000000000, 0.000000000000000000 ) ) ;
#5898 = ORIENTED_EDGE ( 'NONE', *, *, #5704, .T. ) ;
#5899 = DIRECTION ( 'NONE',  ( -0.000000000000000000, -0.000000000000000000, 1.000000000000000000 ) ) ;
#5900 = CARTESIAN_POINT ( 'NONE',  ( 3.580422610670019878, -18.00000000043040771, 4.615668750180310198 ) ) ;
#5901 = VECTOR ( 'NONE', #14744, 1000.000000000000000 ) ;
#5902 = FACE_OUTER_BOUND ( 'NONE', #278, .T. ) ;
#5903 = FACE_OUTER_BOUND ( 'NONE', #15020, .T. ) ;
#5904 = VERTEX_POINT ( 'NONE', #9020 ) ;
#5905 = EDGE_CURVE ( 'NONE', #10495, #12190, #2132, .T. ) ;
#5906 = DIRECTION ( 'NONE',  ( -1.000000000000000000, 0.000000000000000000, 0.000000000000000000 ) ) ;
#5907 = FACE_OUTER_BOUND ( 'NONE', #8644, .T. ) ;
#5908 = EDGE_LOOP ( 'NONE', ( #3174, #18509 ) ) ;
#5909 = CARTESIAN_POINT ( 'NONE',  ( 12.30490414407268851, -19.44545088549631018, -77.05113792083442092 ) ) ;
#5910 = CARTESIAN_POINT ( 'NONE',  ( -24.99999999999999289, -97.49621075554985339, 111.6458212409894486 ) ) ;
#5911 = CARTESIAN_POINT ( 'NONE',  ( -2.163827323447877821E-09, -17.99999999999999645, -4.514799999819691934 ) ) ;
#5912 = ORIENTED_EDGE ( 'NONE', *, *, #13621, .F. ) ;
#5913 = ORIENTED_EDGE ( 'NONE', *, *, #4044, .T. ) ;
#5914 = CARTESIAN_POINT ( 'NONE',  ( 0.000000000000000000, 11.98658579560587789, 64.13855129306472236 ) ) ;
#5915 = AXIS2_PLACEMENT_3D ( 'NONE', #13053, #17930, #16023 ) ;
#5916 = FACE_OUTER_BOUND ( 'NONE', #2888, .T. ) ;
#5917 = CARTESIAN_POINT ( 'NONE',  ( 0.000000000000000000, 0.000000000000000000, -43.00000000000000000 ) ) ;
#5918 = DIRECTION ( 'NONE',  ( -1.000000000000000000, 0.000000000000000000, 0.000000000000000000 ) ) ;
#5919 = CARTESIAN_POINT ( 'NONE',  ( 0.000000000000000000, 0.000000000000000000, 0.000000000000000000 ) ) ;
#5920 = CARTESIAN_POINT ( 'NONE',  ( 16.62983158603122646, 6.888301780572504640, 3.869487500180308182 ) ) ;
#5921 = CARTESIAN_POINT ( 'NONE',  ( 6.929096493489630859, -2.870125743571144472, -21.04723749981969050 ) ) ;
#5922 = ORIENTED_EDGE ( 'NONE', *, *, #13166, .T. ) ;
#5923 = AXIS2_PLACEMENT_3D ( 'NONE', #12821, #17585, #12497 ) ;
#5924 = CARTESIAN_POINT ( 'NONE',  ( 19.99999999999999645, 29.55812890832068973, -65.65300461859658299 ) ) ;
#5925 = CARTESIAN_POINT ( 'NONE',  ( -12.54593441562640166, 8.382925371439625906, 6.293301831519076295 ) ) ;
#5926 = CARTESIAN_POINT ( 'NONE',  ( 85.00002539999999840, 3.872983346207417021, -1.000000000000000000 ) ) ;
#5927 = AXIS2_PLACEMENT_3D ( 'NONE', #18177, #6611, #158 ) ;
#5928 = VERTEX_POINT ( 'NONE', #8904 ) ;
#5929 = ADVANCED_FACE ( 'NONE', ( #10500 ), #13576, .T. ) ;
#5930 = DIRECTION ( 'NONE',  ( 0.000000000000000000, 0.000000000000000000, 1.000000000000000000 ) ) ;
#5931 = CARTESIAN_POINT ( 'NONE',  ( 12.72792206288790950, 12.72792205982780089, -15.56957499981969129 ) ) ;
#5932 = DIRECTION ( 'NONE',  ( -1.000000000000000000, -0.000000000000000000, -0.000000000000000000 ) ) ;
#5933 = ORIENTED_EDGE ( 'NONE', *, *, #7636, .F. ) ;
#5934 = CARTESIAN_POINT ( 'NONE',  ( 6.249999999999902300, -10.82531754730554496, 46.00000000000000711 ) ) ;
#5935 = ORIENTED_EDGE ( 'NONE', *, *, #6120, .F. ) ;
#5936 = DIRECTION ( 'NONE',  ( 0.000000000000000000, 0.000000000000000000, -1.000000000000000000 ) ) ;
#5937 = DIRECTION ( 'NONE',  ( -1.000000000000000000, 0.000000000000000000, 0.000000000000000000 ) ) ;
#5938 = ORIENTED_EDGE ( 'NONE', *, *, #4702, .F. ) ;
#5939 = VERTEX_POINT ( 'NONE', #975 ) ;
#5940 = DIRECTION ( 'NONE',  ( 0.000000000000000000, 0.000000000000000000, 1.000000000000000000 ) ) ;
#5941 = CARTESIAN_POINT ( 'NONE',  ( 0.000000000000000000, 63.85430960833490843, 16.34407078397899582 ) ) ;
#5942 = VECTOR ( 'NONE', #3953, 1000.000000000000000 ) ;
#5943 = FACE_OUTER_BOUND ( 'NONE', #1843, .T. ) ;
#5944 = CARTESIAN_POINT ( 'NONE',  ( -9.015947181032828388E-10, -7.500000000000000888, -25.54494999981968917 ) ) ;
#5945 = FACE_OUTER_BOUND ( 'NONE', #18607, .T. ) ;
#5946 = DIRECTION ( 'NONE',  ( 1.202124453834178339E-10, 1.000000000000000000, -1.511356216916759083E-25 ) ) ;
#5947 = DIRECTION ( 'NONE',  ( 1.000000000000000000, 0.000000000000000000, 0.000000000000000000 ) ) ;
#5948 = ORIENTED_EDGE ( 'NONE', *, *, #18287, .T. ) ;
#5949 = CARTESIAN_POINT ( 'NONE',  ( 0.2500000000000002220, 4.898587196589412829E-16, -4.000000000000000000 ) ) ;
#5950 = VERTEX_POINT ( 'NONE', #12191 ) ;
#5951 = CARTESIAN_POINT ( 'NONE',  ( 2.163825119083639534E-09, 18.00000000000000000, -18.65229999981968589 ) ) ;
#5952 = LINE ( 'NONE', #12647, #15041 ) ;
#5953 = EDGE_LOOP ( 'NONE', ( #15822, #3823 ) ) ;
#5954 = LINE ( 'NONE', #12433, #19422 ) ;
#5955 = AXIS2_PLACEMENT_3D ( 'NONE', #16796, #7041, #16904 ) ;
#5956 = EDGE_LOOP ( 'NONE', ( #6829, #19969, #20262, #8114 ) ) ;
#5957 = CIRCLE ( 'NONE', #8653, 14.49999999999999822 ) ;
#5958 = DIRECTION ( 'NONE',  ( 0.000000000000000000, 0.000000000000000000, 1.000000000000000000 ) ) ;
#5959 = DIRECTION ( 'NONE',  ( -1.000000000000000000, -0.000000000000000000, 0.000000000000000000 ) ) ;
#5960 = CARTESIAN_POINT ( 'NONE',  ( -2.870125741905210415, 6.929096494179677990, -2.571512499819693875 ) ) ;
#5961 = ORIENTED_EDGE ( 'NONE', *, *, #15174, .F. ) ;
#5962 = DIRECTION ( 'NONE',  ( 0.000000000000000000, 0.8878852184023732219, 0.4600650377311559791 ) ) ;
#5963 = EDGE_CURVE ( 'NONE', #1568, #17751, #15378, .T. ) ;
#5964 = ADVANCED_FACE ( 'NONE', ( #8790 ), #13686, .T. ) ;
#5965 = LINE ( 'NONE', #15606, #3595 ) ;
#5966 = CARTESIAN_POINT ( 'NONE',  ( 19.99999999999999645, 64.79224928664392280, 25.14373648582975918 ) ) ;
#5967 = DIRECTION ( 'NONE',  ( 0.000000000000000000, 1.000000000000000000, 0.000000000000000000 ) ) ;
#5968 = CIRCLE ( 'NONE', #6968, 10.85999999999999410 ) ;
#5969 = CARTESIAN_POINT ( 'NONE',  ( -4.248408730893246776, -6.358192987158592047, 13.03864375018031119 ) ) ;
#5970 = EDGE_CURVE ( 'NONE', #15394, #197, #6144, .T. ) ;
#5971 = ORIENTED_EDGE ( 'NONE', *, *, #16157, .F. ) ;
#5972 = AXIS2_PLACEMENT_3D ( 'NONE', #299, #7944, #9935 ) ;
#5973 = AXIS2_PLACEMENT_3D ( 'NONE', #11717, #19654, #14895 ) ;
#5974 = DIRECTION ( 'NONE',  ( -0.000000000000000000, -0.000000000000000000, 1.000000000000000000 ) ) ;
#5975 = CIRCLE ( 'NONE', #2592, 2.649999999999987477 ) ;
#5976 = CARTESIAN_POINT ( 'NONE',  ( 19.99999999999999645, 0.000000000000000000, 0.000000000000000000 ) ) ;
#5977 = EDGE_LOOP ( 'NONE', ( #10687, #4226 ) ) ;
#5978 = DIRECTION ( 'NONE',  ( -1.000000000000000000, -0.000000000000000000, -0.000000000000000000 ) ) ;
#5979 = CARTESIAN_POINT ( 'NONE',  ( 19.99999999999999645, 0.000000000000000000, 0.000000000000000000 ) ) ;
#5980 = ORIENTED_EDGE ( 'NONE', *, *, #9203, .F. ) ;
#5981 = CARTESIAN_POINT ( 'NONE',  ( 6.888301784570728614, 16.62983158437510056, -16.15863749981969377 ) ) ;
#5982 = AXIS2_PLACEMENT_3D ( 'NONE', #13265, #6782, #13164 ) ;
#5983 = CARTESIAN_POINT ( 'NONE',  ( 19.99999999999999645, -36.59093685910587368, -62.00889726308066940 ) ) ;
#5984 = DIRECTION ( 'NONE',  ( -1.000000000000000000, 0.000000000000000000, -0.000000000000000000 ) ) ;
#5985 = ORIENTED_EDGE ( 'NONE', *, *, #13835, .F. ) ;
#5986 = EDGE_CURVE ( 'NONE', #588, #16334, #2979, .T. ) ;
#5987 = CARTESIAN_POINT ( 'NONE',  ( -65.00002539999999840, 3.872983346207417021, -1.000000000000000000 ) ) ;
#5988 = VECTOR ( 'NONE', #10698, 1000.000000000000000 ) ;
#5989 = ORIENTED_EDGE ( 'NONE', *, *, #14052, .T. ) ;
#5990 = DIRECTION ( 'NONE',  ( 0.000000000000000000, 1.000000000000000000, -0.000000000000000000 ) ) ;
#5991 = AXIS2_PLACEMENT_3D ( 'NONE', #18008, #19387, #13038 ) ;
#5992 = VERTEX_POINT ( 'NONE', #20461 ) ;
#5993 = EDGE_CURVE ( 'NONE', #4723, #16392, #18982, .T. ) ;
#5994 = AXIS2_PLACEMENT_3D ( 'NONE', #5138, #5854, #7336 ) ;
#5995 = ADVANCED_FACE ( 'NONE', ( #18885 ), #12412, .T. ) ;
#5996 = DIRECTION ( 'NONE',  ( 0.000000000000000000, -0.5000000000000013323, -0.8660254037844380415 ) ) ;
#5997 = FACE_OUTER_BOUND ( 'NONE', #13404, .T. ) ;
#5998 = VECTOR ( 'NONE', #19078, 1000.000000000000000 ) ;
#5999 = CARTESIAN_POINT ( 'NONE',  ( -13.67243654778936168, -5.663308646854336992, -8.411270581158460047 ) ) ;
#6000 = ORIENTED_EDGE ( 'NONE', *, *, #13718, .T. ) ;
#6001 = FACE_OUTER_BOUND ( 'NONE', #16252, .T. ) ;
#6002 = ORIENTED_EDGE ( 'NONE', *, *, #5189, .T. ) ;
#6003 = DIRECTION ( 'NONE',  ( -1.000000000000000000, 0.000000000000000000, 0.000000000000000000 ) ) ;
#6004 = CIRCLE ( 'NONE', #14815, 2.041999999999999815 ) ;
#6005 = CARTESIAN_POINT ( 'NONE',  ( 6.888301780572505528, -16.62983158603121581, 4.321137500180309843 ) ) ;
#6006 = VECTOR ( 'NONE', #7188, 1000.000000000000000 ) ;
#6007 = CARTESIAN_POINT ( 'NONE',  ( 2.870125743571138255, 6.929096493489627306, -20.24338749981969698 ) ) ;
#6008 = DIRECTION ( 'NONE',  ( 1.000000000000000000, 0.000000000000000000, 0.000000000000000000 ) ) ;
#6009 = EDGE_CURVE ( 'NONE', #20501, #8092, #12839, .T. ) ;
#6010 = ORIENTED_EDGE ( 'NONE', *, *, #13798, .F. ) ;
#6011 = EDGE_CURVE ( 'NONE', #7012, #5684, #10025, .T. ) ;
#6012 = DIRECTION ( 'NONE',  ( -0.4999999999999918954, 0.8660254037844433705, 0.000000000000000000 ) ) ;
#6013 = FACE_OUTER_BOUND ( 'NONE', #6879, .T. ) ;
#6014 = AXIS2_PLACEMENT_3D ( 'NONE', #12484, #13755, #4526 ) ;
#6015 = ORIENTED_EDGE ( 'NONE', *, *, #2600, .T. ) ;
#6016 = DIRECTION ( 'NONE',  ( -1.000000000000000000, -0.000000000000000000, -0.000000000000000000 ) ) ;
#6017 = DIRECTION ( 'NONE',  ( 1.000000000000000000, 1.836909530733573776E-16, 0.000000000000000000 ) ) ;
#6018 = CARTESIAN_POINT ( 'NONE',  ( -10.19618095047497874, 15.25966317163202746, -10.11089374981968803 ) ) ;
#6019 = AXIS2_PLACEMENT_3D ( 'NONE', #17655, #14781, #9699 ) ;
#6020 = EDGE_CURVE ( 'NONE', #3970, #19211, #11133, .T. ) ;
#6021 = ORIENTED_EDGE ( 'NONE', *, *, #5069, .T. ) ;
#6022 = LINE ( 'NONE', #15769, #13437 ) ;
#6023 = AXIS2_PLACEMENT_3D ( 'NONE', #1588, #4857, #11327 ) ;
#6024 = CARTESIAN_POINT ( 'NONE',  ( 19.99999999999999645, 10.77748419466696284, 63.93680186330476545 ) ) ;
#6025 = DIRECTION ( 'NONE',  ( 0.000000000000000000, 0.000000000000000000, 1.000000000000000000 ) ) ;
#6026 = LINE ( 'NONE', #14511, #12610 ) ;
#6027 = CARTESIAN_POINT ( 'NONE',  ( 6.250000000000200728, 10.82531754730537621, 34.39999999999999858 ) ) ;
#6028 = CARTESIAN_POINT ( 'NONE',  ( 6.888301780572508193, -16.62983158603122291, 6.225737500180309247 ) ) ;
#6029 = FACE_OUTER_BOUND ( 'NONE', #4177, .T. ) ;
#6030 = EDGE_LOOP ( 'NONE', ( #718, #7106, #9632, #6000, #12254, #17389 ) ) ;
#6031 = CARTESIAN_POINT ( 'NONE',  ( -30.00000000000000000, -125.0000000000000000, 90.00000000000002842 ) ) ;
#6032 = CARTESIAN_POINT ( 'NONE',  ( -10.46442989454075168, -10.46442989202483709, 4.231583081519074696 ) ) ;
#6033 = DIRECTION ( 'NONE',  ( 0.000000000000000000, 0.000000000000000000, 1.000000000000000000 ) ) ;
#6034 = ORIENTED_EDGE ( 'NONE', *, *, #17781, .F. ) ;
#6035 = CARTESIAN_POINT ( 'NONE',  ( 0.3263565795980677420, -4.430380094434308802, -0.2484800633750392507 ) ) ;
#6036 = CARTESIAN_POINT ( 'NONE',  ( 15.25966316918061416, -10.19618095414378622, -13.50785624981968880 ) ) ;
#6037 = LINE ( 'NONE', #12509, #2615 ) ;
#6038 = ORIENTED_EDGE ( 'NONE', *, *, #14554, .T. ) ;
#6039 = CARTESIAN_POINT ( 'NONE',  ( -7.500000000000004441, 9.706494107352906755E-15, -23.18869999999769860 ) ) ;
#6040 = ORIENTED_EDGE ( 'NONE', *, *, #19319, .T. ) ;
#6041 = CARTESIAN_POINT ( 'NONE',  ( 33.28744621271695792, -29.52989836050402772, -73.00509023842178635 ) ) ;
#6042 = CARTESIAN_POINT ( 'NONE',  ( 19.99999999999999645, 0.000000000000000000, 0.000000000000000000 ) ) ;
#6043 = VERTEX_POINT ( 'NONE', #9535 ) ;
#6044 = ORIENTED_EDGE ( 'NONE', *, *, #6381, .T. ) ;
#6045 = CARTESIAN_POINT ( 'NONE',  ( 30.84620721615401351, -110.7731078431028777, -73.91085715544664936 ) ) ;
#6046 = CARTESIAN_POINT ( 'NONE',  ( 50.00000000000000000, 31.35083268962917558, 84.99999999999998579 ) ) ;
#6047 = ADVANCED_FACE ( 'NONE', ( #7521 ), #15794, .F. ) ;
#6048 = EDGE_CURVE ( 'NONE', #2608, #14851, #17395, .T. ) ;
#6049 = CARTESIAN_POINT ( 'NONE',  ( 2.500000000000000000, -1.768423874527823569, 1.021000000000002350 ) ) ;
#6050 = CARTESIAN_POINT ( 'NONE',  ( -7.902369978624323110, -7.902369976724391343, 12.90426524971319999 ) ) ;
#6051 = CARTESIAN_POINT ( 'NONE',  ( 19.99999999999999645, 23.08379033237351052, 61.02926039941442582 ) ) ;
#6052 = DIRECTION ( 'NONE',  ( 0.8191520442889896891, 1.003171929053522158E-16, -0.5735764363510490460 ) ) ;
#6053 = CARTESIAN_POINT ( 'NONE',  ( 0.000000000000000000, 27.80658314415319055, -66.41380830714092554 ) ) ;
#6054 = ORIENTED_EDGE ( 'NONE', *, *, #12607, .F. ) ;
#6055 = DIRECTION ( 'NONE',  ( -1.000000000000000000, 0.000000000000000000, 0.000000000000000000 ) ) ;
#6056 = ORIENTED_EDGE ( 'NONE', *, *, #11617, .T. ) ;
#6057 = CARTESIAN_POINT ( 'NONE',  ( 6.888301784570728614, 16.62983158437510056, -8.638237499819689802 ) ) ;
#6058 = LINE ( 'NONE', #12532, #3212 ) ;
#6059 = ORIENTED_EDGE ( 'NONE', *, *, #17772, .T. ) ;
#6060 = DIRECTION ( 'NONE',  ( 1.000000000000000000, -0.000000000000000000, -0.000000000000000000 ) ) ;
#6061 = EDGE_LOOP ( 'NONE', ( #394, #8047, #5938, #9208 ) ) ;
#6062 = CARTESIAN_POINT ( 'NONE',  ( 0.000000000000000000, 54.08351995568756365, -35.76369202524444546 ) ) ;
#6063 = CYLINDRICAL_SURFACE ( 'NONE', #9071, 27.60000000002759890 ) ;
#6064 = DIRECTION ( 'NONE',  ( 1.000000000000000000, 0.000000000000000000, 0.000000000000000000 ) ) ;
#6065 = VERTEX_POINT ( 'NONE', #14006 ) ;
#6066 = DIRECTION ( 'NONE',  ( -0.000000000000000000, -0.000000000000000000, 1.000000000000000000 ) ) ;
#6067 = DIRECTION ( 'NONE',  ( 0.000000000000000000, 0.000000000000000000, 1.000000000000000000 ) ) ;
#6068 = CARTESIAN_POINT ( 'NONE',  ( 19.99999999999999645, -38.22257254261781867, 61.01667762370124137 ) ) ;
#6069 = DIRECTION ( 'NONE',  ( 0.000000000000000000, 0.1361666490962400722, 0.9906859460363316439 ) ) ;
#6070 = DIRECTION ( 'NONE',  ( -0.000000000000000000, -0.000000000000000000, -1.000000000000000000 ) ) ;
#6071 = ORIENTED_EDGE ( 'NONE', *, *, #2647, .T. ) ;
#6072 = CARTESIAN_POINT ( 'NONE',  ( 19.99999999999999645, 38.69327817041775575, 52.53819777490647880 ) ) ;
#6073 = DIRECTION ( 'NONE',  ( 1.000000000000000000, 0.000000000000000000, 0.000000000000000000 ) ) ;
#6074 = EDGE_LOOP ( 'NONE', ( #6251, #12877, #16998, #644 ) ) ;
#6075 = EDGE_CURVE ( 'NONE', #13895, #19557, #6640, .T. ) ;
#6076 = DIRECTION ( 'NONE',  ( 0.000000000000000000, -1.224646799147354686E-16, 1.000000000000000000 ) ) ;
#6077 = DIRECTION ( 'NONE',  ( -1.000000000000000000, 0.000000000000000000, -0.000000000000000000 ) ) ;
#6078 = EDGE_CURVE ( 'NONE', #8357, #18441, #19283, .T. ) ;
#6079 = VERTEX_POINT ( 'NONE', #9441 ) ;
#6080 = CARTESIAN_POINT ( 'NONE',  ( 12.72792205982779734, -12.72792206288791128, -22.63832499981969093 ) ) ;
#6081 = CARTESIAN_POINT ( 'NONE',  ( 2.500000000000000000, 1.768423874527822459, -1.021000000000002794 ) ) ;
#6082 = CARTESIAN_POINT ( 'NONE',  ( 19.99999999999999645, 0.000000000000000000, 0.000000000000000000 ) ) ;
#6083 = VERTEX_POINT ( 'NONE', #15897 ) ;
#6084 = DIRECTION ( 'NONE',  ( 0.000000000000000000, 0.000000000000000000, -1.000000000000000000 ) ) ;
#6085 = ORIENTED_EDGE ( 'NONE', *, *, #13384, .F. ) ;
#6086 = DIRECTION ( 'NONE',  ( -1.000000000000000000, -0.000000000000000000, -0.000000000000000000 ) ) ;
#6087 = EDGE_CURVE ( 'NONE', #4783, #6177, #7842, .T. ) ;
#6088 = ORIENTED_EDGE ( 'NONE', *, *, #4753, .T. ) ;
#6089 = EDGE_CURVE ( 'NONE', #16461, #15306, #9018, .T. ) ;
#6090 = DIRECTION ( 'NONE',  ( -1.000000000000000000, 0.000000000000000000, 0.000000000000000000 ) ) ;
#6091 = FACE_OUTER_BOUND ( 'NONE', #14925, .T. ) ;
#6092 = CARTESIAN_POINT ( 'NONE',  ( -1.779019326032424922E-09, -14.79893867758297610, -10.17845808115846218 ) ) ;
#6093 = ORIENTED_EDGE ( 'NONE', *, *, #8322, .T. ) ;
#6094 = DIRECTION ( 'NONE',  ( -1.000000000000000000, 0.000000000000000000, 0.000000000000000000 ) ) ;
#6095 = DIRECTION ( 'NONE',  ( -0.000000000000000000, -0.000000000000000000, 1.000000000000000000 ) ) ;
#6096 = ORIENTED_EDGE ( 'NONE', *, *, #16474, .T. ) ;
#6097 = CARTESIAN_POINT ( 'NONE',  ( 18.81636376335696426, -10.41831967068597997, 83.08843782764408559 ) ) ;
#6098 = EDGE_CURVE ( 'NONE', #12564, #3220, #16147, .T. ) ;
#6099 = CARTESIAN_POINT ( 'NONE',  ( -3.580422614997674557, -17.99999999956957808, 14.62973125018031162 ) ) ;
#6100 = EDGE_CURVE ( 'NONE', #6425, #8357, #13089, .T. ) ;
#6101 = CARTESIAN_POINT ( 'NONE',  ( 0.000000000000000000, 0.000000000000000000, 0.000000000000000000 ) ) ;
#6102 = CIRCLE ( 'NONE', #6775, 5.000000000000000888 ) ;
#6103 = FACE_OUTER_BOUND ( 'NONE', #11895, .T. ) ;
#6104 = ORIENTED_EDGE ( 'NONE', *, *, #19458, .T. ) ;
#6105 = EDGE_CURVE ( 'NONE', #14994, #9313, #414, .T. ) ;
#6106 = DIRECTION ( 'NONE',  ( -0.000000000000000000, -0.000000000000000000, 1.000000000000000000 ) ) ;
#6107 = CARTESIAN_POINT ( 'NONE',  ( 30.00000000000000000, -99.99999999999998579, -52.00000000000000000 ) ) ;
#6108 = VECTOR ( 'NONE', #4587, 1000.000000000000000 ) ;
#6109 = ORIENTED_EDGE ( 'NONE', *, *, #7606, .F. ) ;
#6110 = CARTESIAN_POINT ( 'NONE',  ( 0.000000000000000000, 29.55812890832068973, -65.65300461859658299 ) ) ;
#6111 = CARTESIAN_POINT ( 'NONE',  ( 6.358192987158592047, -4.248408730893246776, 1.257393750180309189 ) ) ;
#6112 = CARTESIAN_POINT ( 'NONE',  ( -6.888301784570736608, -16.62983158437509346, -3.925737499819691223 ) ) ;
#6113 = EDGE_LOOP ( 'NONE', ( #18219, #15998, #11005, #16724 ) ) ;
#6114 = DIRECTION ( 'NONE',  ( 1.000000000000000000, 1.836909530733573776E-16, 0.000000000000000000 ) ) ;
#6115 = FACE_BOUND ( 'NONE', #9162, .T. ) ;
#6116 = CIRCLE ( 'NONE', #17973, 7.500000000000000000 ) ;
#6117 = DIRECTION ( 'NONE',  ( 1.000000000000000000, 0.000000000000000000, 0.000000000000000000 ) ) ;
#6118 = CARTESIAN_POINT ( 'NONE',  ( 0.000000000000000000, 10.74906464462217848, -71.19310085447958159 ) ) ;
#6119 = DIRECTION ( 'NONE',  ( -1.000000000000000000, 0.000000000000000000, -6.982962677686266711E-15 ) ) ;
#6120 = EDGE_CURVE ( 'NONE', #1182, #3247, #20870, .T. ) ;
#6121 = CARTESIAN_POINT ( 'NONE',  ( 3.580422610670021211, -18.00000000043041481, 6.520268750180309603 ) ) ;
#6122 = EDGE_CURVE ( 'NONE', #18991, #12032, #7319, .T. ) ;
#6123 = DIRECTION ( 'NONE',  ( -0.000000000000000000, -0.000000000000000000, 1.000000000000000000 ) ) ;
#6124 = CIRCLE ( 'NONE', #17978, 27.60000000002760245 ) ;
#6125 = ORIENTED_EDGE ( 'NONE', *, *, #5986, .T. ) ;
#6126 = DIRECTION ( 'NONE',  ( -1.000000000000000000, 0.000000000000000000, 0.000000000000000000 ) ) ;
#6127 = CARTESIAN_POINT ( 'NONE',  ( 12.54593441764186679, 8.382925368423272516, 18.66361433151907079 ) ) ;
#6128 = ADVANCED_FACE ( 'NONE', ( #1801 ), #8254, .T. ) ;
#6129 = CARTESIAN_POINT ( 'NONE',  ( 19.99999999999999645, -63.05226888949880504, -15.11556105343524514 ) ) ;
#6130 = ORIENTED_EDGE ( 'NONE', *, *, #672, .F. ) ;
#6131 = ADVANCED_BREP_SHAPE_REPRESENTATION ( '', ( #10450, #12461 ), #2252 ) ;
#6132 = FACE_OUTER_BOUND ( 'NONE', #17937, .T. ) ;
#6133 = CYLINDRICAL_SURFACE ( 'NONE', #10043, 11.50000000000000000 ) ;
#6134 = CYLINDRICAL_SURFACE ( 'NONE', #12786, 2.099999999999997868 ) ;
#6135 = EDGE_LOOP ( 'NONE', ( #16412, #5737, #3915, #15562 ) ) ;
#6136 = DIRECTION ( 'NONE',  ( 0.000000000000000000, 0.000000000000000000, -1.000000000000000000 ) ) ;
#6137 = VECTOR ( 'NONE', #1031, 1000.000000000000000 ) ;
#6138 = ORIENTED_EDGE ( 'NONE', *, *, #1346, .F. ) ;
#6139 = CARTESIAN_POINT ( 'NONE',  ( -30.00000000000000000, -49.99999999999997868, 71.93747284969079203 ) ) ;
#6140 = DIRECTION ( 'NONE',  ( -0.000000000000000000, -0.000000000000000000, -1.000000000000000000 ) ) ;
#6141 = ORIENTED_EDGE ( 'NONE', *, *, #14421, .T. ) ;
#6142 = AXIS2_PLACEMENT_3D ( 'NONE', #403, #15135, #7066 ) ;
#6143 = ORIENTED_EDGE ( 'NONE', *, *, #16419, .F. ) ;
#6144 = LINE ( 'NONE', #12736, #20524 ) ;
#6145 = AXIS2_PLACEMENT_3D ( 'NONE', #9760, #17718, #7965 ) ;
#6146 = DIRECTION ( 'NONE',  ( 0.000000000000000000, 0.8878852184023764416, -0.4600650377311500394 ) ) ;
#6147 = DIRECTION ( 'NONE',  ( -1.000000000000000000, -0.000000000000000000, -0.000000000000000000 ) ) ;
#6148 = CARTESIAN_POINT ( 'NONE',  ( 11.17563879704982632, -2.222972771497745637, -11.48785899935257504 ) ) ;
#6149 = AXIS2_PLACEMENT_3D ( 'NONE', #1372, #7724, #7817 ) ;
#6150 = CARTESIAN_POINT ( 'NONE',  ( 2.870125741905211747, -6.929096494179675325, -26.13401249981968988 ) ) ;
#6151 = CARTESIAN_POINT ( 'NONE',  ( 0.000000000000000000, 65.23577793412344761, -1.313498510941930153 ) ) ;
#6152 = AXIS2_PLACEMENT_3D ( 'NONE', #3680, #2312, #5475 ) ;
#6153 = DIRECTION ( 'NONE',  ( 0.000000000000000000, 0.000000000000000000, -1.000000000000000000 ) ) ;
#6154 = CARTESIAN_POINT ( 'NONE',  ( -24.99999999999999289, 31.35083268962909742, -2.067608244099269852E-13 ) ) ;
#6155 = ORIENTED_EDGE ( 'NONE', *, *, #5589, .F. ) ;
#6156 = CARTESIAN_POINT ( 'NONE',  ( 2.500000000000000000, -1.178949249685213863, 2.042000000000002924 ) ) ;
#6157 = ORIENTED_EDGE ( 'NONE', *, *, #15380, .T. ) ;
#6158 = CARTESIAN_POINT ( 'NONE',  ( -6.888301780572501976, 16.62983158603122291, -19.24136249981968660 ) ) ;
#6159 = CARTESIAN_POINT ( 'NONE',  ( 19.99999999999999645, 36.59093685910711002, -62.00889726307995176 ) ) ;
#6160 = ORIENTED_EDGE ( 'NONE', *, *, #19954, .T. ) ;
#6161 = CARTESIAN_POINT ( 'NONE',  ( 9.999999999999998224, -18.50424539729892714, 69.58155576219110117 ) ) ;
#6162 = ORIENTED_EDGE ( 'NONE', *, *, #9944, .T. ) ;
#6163 = DIRECTION ( 'NONE',  ( 0.000000000000000000, 0.000000000000000000, -1.000000000000000000 ) ) ;
#6164 = CARTESIAN_POINT ( 'NONE',  ( 0.000000000000000000, 0.000000000000000000, 40.00000000000000000 ) ) ;
#6165 = CARTESIAN_POINT ( 'NONE',  ( -31.75000000000000000, -10.85999999999999410, 1.329966423874024955E-15 ) ) ;
#6166 = EDGE_CURVE ( 'NONE', #2187, #1411, #8683, .T. ) ;
#6167 = VERTEX_POINT ( 'NONE', #19692 ) ;
#6168 = FACE_OUTER_BOUND ( 'NONE', #19328, .T. ) ;
#6169 = CIRCLE ( 'NONE', #19700, 27.60000000002759890 ) ;
#6170 = CIRCLE ( 'NONE', #15638, 17.50000000000000355 ) ;
#6171 = AXIS2_PLACEMENT_3D ( 'NONE', #10566, #11939, #13443 ) ;
#6172 = DIRECTION ( 'NONE',  ( -1.000000000000000000, 0.000000000000000000, 0.000000000000000000 ) ) ;
#6173 = CARTESIAN_POINT ( 'NONE',  ( -16.62983158603121936, -6.888301780572499311, -21.59761249981969300 ) ) ;
#6174 = DIRECTION ( 'NONE',  ( -0.5000000000000037748, -0.8660254037844364872, 0.000000000000000000 ) ) ;
#6175 = DIRECTION ( 'NONE',  ( 1.000000000000000000, 0.000000000000000000, 0.000000000000000000 ) ) ;
#6176 = AXIS2_PLACEMENT_3D ( 'NONE', #2301, #19890, #10350 ) ;
#6177 = VERTEX_POINT ( 'NONE', #13238 ) ;
#6178 = LINE ( 'NONE', #17746, #17456 ) ;
#6179 = CYLINDRICAL_SURFACE ( 'NONE', #9498, 2.099999999999999645 ) ;
#6180 = VERTEX_POINT ( 'NONE', #18115 ) ;
#6181 = AXIS2_PLACEMENT_3D ( 'NONE', #606, #9077, #1022 ) ;
#6182 = CARTESIAN_POINT ( 'NONE',  ( -44.00000000000000000, -85.00000000000000000, 11.49999999999998579 ) ) ;
#6183 = CARTESIAN_POINT ( 'NONE',  ( 0.000000000000000000, 0.000000000000000000, 46.00000000000000711 ) ) ;
#6184 = AXIS2_PLACEMENT_3D ( 'NONE', #1594, #12614, #19076 ) ;
#6185 = VECTOR ( 'NONE', #14010, 1000.000000000000000 ) ;
#6186 = ORIENTED_EDGE ( 'NONE', *, *, #18434, .T. ) ;
#6187 = CARTESIAN_POINT ( 'NONE',  ( -17.99999999956958519, 3.580422614997674113, -18.80941874981969164 ) ) ;
#6188 = CIRCLE ( 'NONE', #6513, 65.24900000006525147 ) ;
#6189 = DIRECTION ( 'NONE',  ( -1.000000000000000000, -0.000000000000000000, -0.000000000000000000 ) ) ;
#6190 = LINE ( 'NONE', #5880, #18085 ) ;
#6191 = ORIENTED_EDGE ( 'NONE', *, *, #4642, .T. ) ;
#6192 = FACE_OUTER_BOUND ( 'NONE', #5757, .T. ) ;
#6193 = ORIENTED_EDGE ( 'NONE', *, *, #6478, .T. ) ;
#6194 = CARTESIAN_POINT ( 'NONE',  ( 19.99999999999999645, 23.08379033237438094, -61.02926039941409897 ) ) ;
#6195 = EDGE_CURVE ( 'NONE', #18697, #10983, #1914, .T. ) ;
#6196 = VERTEX_POINT ( 'NONE', #308 ) ;
#6197 = CYLINDRICAL_SURFACE ( 'NONE', #5331, 65.24900000006525147 ) ;
#6198 = ADVANCED_FACE ( 'NONE', ( #13147 ), #5171, .F. ) ;
#6199 = AXIS2_PLACEMENT_3D ( 'NONE', #262, #16264, #10007 ) ;
#6200 = EDGE_CURVE ( 'NONE', #20704, #4938, #18167, .T. ) ;
#6201 = AXIS2_PLACEMENT_3D ( 'NONE', #3525, #16460, #17757 ) ;
#6202 = DIRECTION ( 'NONE',  ( -0.000000000000000000, -0.000000000000000000, -1.000000000000000000 ) ) ;
#6203 = CARTESIAN_POINT ( 'NONE',  ( -6.330490856366295382, 9.474249098604511587, 22.67776600064743064 ) ) ;
#6204 = ORIENTED_EDGE ( 'NONE', *, *, #5540, .T. ) ;
#6205 = DIRECTION ( 'NONE',  ( 0.000000000000000000, 0.000000000000000000, 1.000000000000000000 ) ) ;
#6206 = DIRECTION ( 'NONE',  ( -1.000000000000000000, 0.000000000000000000, 0.000000000000000000 ) ) ;
#6207 = VERTEX_POINT ( 'NONE', #3581 ) ;
#6208 = AXIS2_PLACEMENT_3D ( 'NONE', #20458, #5937, #12408 ) ;
#6209 = CARTESIAN_POINT ( 'NONE',  ( 15.31456654470125400, -15.09377138507804972, 79.61049916633108126 ) ) ;
#6210 = AXIS2_PLACEMENT_3D ( 'NONE', #13381, #15170, #977 ) ;
#6211 = DIRECTION ( 'NONE',  ( 1.000000000000000000, -0.000000000000000000, -0.000000000000000000 ) ) ;
#6212 = AXIS2_PLACEMENT_3D ( 'NONE', #2126, #19714, #743 ) ;
#6213 = ORIENTED_EDGE ( 'NONE', *, *, #14819, .F. ) ;
#6214 = DIRECTION ( 'NONE',  ( 0.000000000000000000, 0.000000000000000000, 1.000000000000000000 ) ) ;
#6215 = ORIENTED_EDGE ( 'NONE', *, *, #15063, .T. ) ;
#6216 = DIRECTION ( 'NONE',  ( -1.000000000000000000, 0.000000000000000000, 0.000000000000000000 ) ) ;
#6217 = CARTESIAN_POINT ( 'NONE',  ( -7.500000000000000888, -3.289131931895657122E-15, 5.086300000002307087 ) ) ;
#6218 = CARTESIAN_POINT ( 'NONE',  ( 2.163825119083639120E-09, 17.99999999999999645, -9.227299999819690512 ) ) ;
#6219 = CIRCLE ( 'NONE', #14690, 54.99999999999999289 ) ;
#6220 = VERTEX_POINT ( 'NONE', #3377 ) ;
#6221 = CARTESIAN_POINT ( 'NONE',  ( 19.99999999999999645, -64.52323195238632536, 6.389157729492951354 ) ) ;
#6222 = CIRCLE ( 'NONE', #16376, 27.60000000002759890 ) ;
#6223 = EDGE_CURVE ( 'NONE', #2292, #7786, #5068, .T. ) ;
#6224 = DIRECTION ( 'NONE',  ( -1.000000000000000000, -0.000000000000000000, -0.000000000000000000 ) ) ;
#6225 = EDGE_CURVE ( 'NONE', #12867, #5525, #11733, .T. ) ;
#6226 = DIRECTION ( 'NONE',  ( 0.000000000000000000, 0.000000000000000000, -1.000000000000000000 ) ) ;
#6227 = DIRECTION ( 'NONE',  ( -1.000000000000000000, -0.000000000000000000, -0.000000000000000000 ) ) ;
#6228 = DIRECTION ( 'NONE',  ( -1.000000000000000000, 0.000000000000000000, -6.982962677686266711E-15 ) ) ;
#6229 = CARTESIAN_POINT ( 'NONE',  ( -3.580422614997675890, -17.99999999956958519, 7.109331250180310313 ) ) ;
#6230 = AXIS2_PLACEMENT_3D ( 'NONE', #3711, #13383, #15268 ) ;
#6231 = CIRCLE ( 'NONE', #5213, 7.567219999999999835 ) ;
#6232 = CARTESIAN_POINT ( 'NONE',  ( 0.000000000000000000, 0.000000000000000000, 169.0000000000000000 ) ) ;
#6233 = EDGE_CURVE ( 'NONE', #5196, #7047, #13768, .T. ) ;
#6234 = ORIENTED_EDGE ( 'NONE', *, *, #585, .F. ) ;
#6235 = CARTESIAN_POINT ( 'NONE',  ( -30.00000000000000000, 36.35083268962920044, -90.00000000000000000 ) ) ;
#6236 = CARTESIAN_POINT ( 'NONE',  ( 7.902369976724389566, -7.902369978624323110, -27.15198475028680392 ) ) ;
#6237 = DIRECTION ( 'NONE',  ( -1.000000000000000000, -0.000000000000000000, -0.000000000000000000 ) ) ;
#6238 = CIRCLE ( 'NONE', #3189, 2.650000000000000355 ) ;
#6239 = VERTEX_POINT ( 'NONE', #16522 ) ;
#6240 = CARTESIAN_POINT ( 'NONE',  ( 19.99999999999999645, -36.54710069451017063, -54.05313526368150434 ) ) ;
#6241 = CARTESIAN_POINT ( 'NONE',  ( -15.25966316918061771, 10.19618095414378622, -18.22035624981968738 ) ) ;
#6242 = CARTESIAN_POINT ( 'NONE',  ( 21.18805271706017024, -3.649167310370820871, 90.00000000000000000 ) ) ;
#6243 = EDGE_LOOP ( 'NONE', ( #223, #15604, #16970, #12922 ) ) ;
#6244 = EDGE_CURVE ( 'NONE', #17375, #18530, #8150, .T. ) ;
#6245 = DIRECTION ( 'NONE',  ( -1.000000000000000000, -0.000000000000000000, 0.000000000000000000 ) ) ;
#6246 = VERTEX_POINT ( 'NONE', #7070 ) ;
#6247 = AXIS2_PLACEMENT_3D ( 'NONE', #16635, #8782, #12085 ) ;
#6248 = CARTESIAN_POINT ( 'NONE',  ( 19.99999999999999645, -64.79224928664389438, -2.456263514198281150 ) ) ;
#6249 = CARTESIAN_POINT ( 'NONE',  ( 2.500000000000000000, 0.000000000000000000, 0.000000000000000000 ) ) ;
#6250 = VERTEX_POINT ( 'NONE', #19797 ) ;
#6251 = ORIENTED_EDGE ( 'NONE', *, *, #13780, .F. ) ;
#6252 = CARTESIAN_POINT ( 'NONE',  ( 45.22159793441011999, -8.673994507468391291, -78.07221698934968401 ) ) ;
#6253 = EDGE_CURVE ( 'NONE', #2005, #10676, #18503, .T. ) ;
#6254 = EDGE_CURVE ( 'NONE', #15415, #20612, #7743, .T. ) ;
#6255 = AXIS2_PLACEMENT_3D ( 'NONE', #18958, #19265, #6119 ) ;
#6256 = CARTESIAN_POINT ( 'NONE',  ( 50.00000000000000000, 36.35083268962917202, 90.00000000000000000 ) ) ;
#6257 = EDGE_CURVE ( 'NONE', #9751, #10364, #18427, .T. ) ;
#6258 = CARTESIAN_POINT ( 'NONE',  ( -30.00000000000000000, 36.35083268962920044, -90.00000000000000000 ) ) ;
#6259 = CARTESIAN_POINT ( 'NONE',  ( -10.32494394706616703, 4.276731815070943910, -6.480827749352571665 ) ) ;
#6260 =( GEOMETRIC_REPRESENTATION_CONTEXT ( 3 ) GLOBAL_UNCERTAINTY_ASSIGNED_CONTEXT ( ( #13462 ) ) GLOBAL_UNIT_ASSIGNED_CONTEXT ( ( #3645, #10218, #13414 ) ) REPRESENTATION_CONTEXT ( 'NONE', 'WORKASPACE' ) );
#6261 = CARTESIAN_POINT ( 'NONE',  ( -9.474249097082497073, 6.330490858644137298, 14.96598399971320070 ) ) ;
#6262 = DIRECTION ( 'NONE',  ( 1.000000000000000000, 0.000000000000000000, 0.000000000000000000 ) ) ;
#6263 = CARTESIAN_POINT ( 'NONE',  ( 0.000000000000000000, -43.56693332842751687, -48.57318520917550586 ) ) ;
#6264 = DIRECTION ( 'NONE',  ( 0.000000000000000000, -0.8169698930104470902, 0.5766803221148600889 ) ) ;
#6265 = VERTEX_POINT ( 'NONE', #3783 ) ;
#6266 = DIRECTION ( 'NONE',  ( 0.000000000000000000, 0.000000000000000000, 1.000000000000000000 ) ) ;
#6267 = ORIENTED_EDGE ( 'NONE', *, *, #20217, .T. ) ;
#6268 = CARTESIAN_POINT ( 'NONE',  ( -12.72792206288791128, -12.72792205982779912, -12.76167499981968945 ) ) ;
#6269 = CARTESIAN_POINT ( 'NONE',  ( 19.99999999999999645, 43.56693332842851873, -48.57318520917461058 ) ) ;
#6270 = PRODUCT_DEFINITION_FORMATION_WITH_SPECIFIED_SOURCE ( 'ANY', '', #6770, .NOT_KNOWN. ) ;
#6271 = ORIENTED_EDGE ( 'NONE', *, *, #8978, .F. ) ;
#6272 = EDGE_CURVE ( 'NONE', #3394, #7841, #6967, .T. ) ;
#6273 = CARTESIAN_POINT ( 'NONE',  ( 8.900000000000053646, 10.82531754730546147, 43.00000000000000000 ) ) ;
#6274 = VERTEX_POINT ( 'NONE', #18537 ) ;
#6275 = CARTESIAN_POINT ( 'NONE',  ( -2.870125743571141808, -6.929096493489625530, -6.105887499819693254 ) ) ;
#6276 = DIRECTION ( 'NONE',  ( 0.000000000000000000, -0.000000000000000000, -1.000000000000000000 ) ) ;
#6277 = CARTESIAN_POINT ( 'NONE',  ( 2.870125743571138255, 6.929096493489627306, -1.393387499819692010 ) ) ;
#6278 = VERTEX_POINT ( 'NONE', #18631 ) ;
#6279 = CARTESIAN_POINT ( 'NONE',  ( 2.500000000000000000, 1.768423874527824902, 1.020999999999999019 ) ) ;
#6280 = AXIS2_PLACEMENT_3D ( 'NONE', #17542, #4801, #1114 ) ;
#6281 = CARTESIAN_POINT ( 'NONE',  ( -3.580422614997674557, -17.99999999956957808, -23.07026874981969300 ) ) ;
#6282 = DIRECTION ( 'NONE',  ( -1.000000000000000000, 0.000000000000000000, 0.000000000000000000 ) ) ;
#6283 = CARTESIAN_POINT ( 'NONE',  ( 2.870125741905212635, -6.929096494179677101, 11.56598750018030941 ) ) ;
#6284 = EDGE_LOOP ( 'NONE', ( #365, #19352, #3238, #8745 ) ) ;
#6285 = DIRECTION ( 'NONE',  ( 1.000000000000000000, 0.000000000000000000, 0.000000000000000000 ) ) ;
#6286 = EDGE_CURVE ( 'NONE', #18936, #20567, #8559, .T. ) ;
#6287 = AXIS2_PLACEMENT_3D ( 'NONE', #1873, #282, #8329 ) ;
#6288 = CARTESIAN_POINT ( 'NONE',  ( 19.99999999999999645, 0.000000000000000000, 0.000000000000000000 ) ) ;
#6289 = EDGE_LOOP ( 'NONE', ( #3729, #12474, #997, #9876 ) ) ;
#6290 = DIRECTION ( 'NONE',  ( -1.000000000000000000, 0.000000000000000000, 0.000000000000000000 ) ) ;
#6291 = CARTESIAN_POINT ( 'NONE',  ( -15.15000000000000568, 3.245314017740485469E-16, 43.00000000000000000 ) ) ;
#6292 = AXIS2_PLACEMENT_3D ( 'NONE', #19291, #4775, #17720 ) ;
#6293 = ORIENTED_EDGE ( 'NONE', *, *, #15852, .F. ) ;
#6294 = DIRECTION ( 'NONE',  ( 0.000000000000000000, 0.000000000000000000, -1.000000000000000000 ) ) ;
#6295 = DIRECTION ( 'NONE',  ( 0.000000000000000000, 0.000000000000000000, 1.000000000000000000 ) ) ;
#6296 = DIRECTION ( 'NONE',  ( -1.000000000000000000, 0.000000000000000000, 0.000000000000000000 ) ) ;
#6297 = EDGE_LOOP ( 'NONE', ( #12035, #19587, #11065, #5751, #20058 ) ) ;
#6298 = CARTESIAN_POINT ( 'NONE',  ( 17.50000000000000355, 2.143131898507868643E-15, 43.00000000000000000 ) ) ;
#6299 = ORIENTED_EDGE ( 'NONE', *, *, #14660, .F. ) ;
#6300 = CYLINDRICAL_SURFACE ( 'NONE', #7849, 10.00000000000000178 ) ;
#6301 = ORIENTED_EDGE ( 'NONE', *, *, #13988, .T. ) ;
#6302 = AXIS2_PLACEMENT_3D ( 'NONE', #18140, #8279, #3403 ) ;
#6303 = DIRECTION ( 'NONE',  ( -1.000000000000000000, -0.000000000000000000, -0.000000000000000000 ) ) ;
#6304 = AXIS2_PLACEMENT_3D ( 'NONE', #6724, #10227, #15001 ) ;
#6305 = VECTOR ( 'NONE', #12807, 1000.000000000000000 ) ;
#6306 = DIRECTION ( 'NONE',  ( -1.000000000000000000, 0.000000000000000000, -0.000000000000000000 ) ) ;
#6307 = CARTESIAN_POINT ( 'NONE',  ( -10.32494394706616703, 4.276731815070943910, 21.79417225064743135 ) ) ;
#6308 = ADVANCED_FACE ( 'NONE', ( #3889 ), #10370, .F. ) ;
#6309 = ORIENTED_EDGE ( 'NONE', *, *, #12781, .T. ) ;
#6310 = CARTESIAN_POINT ( 'NONE',  ( 0.000000000000000000, 63.05226888949912478, -15.11556105343395906 ) ) ;
#6311 = ADVANCED_FACE ( 'NONE', ( #13456 ), #20106, .F. ) ;
#6312 = AXIS2_PLACEMENT_3D ( 'NONE', #8813, #7337, #8613 ) ;
#6313 = DIRECTION ( 'NONE',  ( 0.000000000000000000, 0.3984010898462361783, 0.9172113015054552676 ) ) ;
#6314 = ORIENTED_EDGE ( 'NONE', *, *, #2347, .T. ) ;
#6315 = CARTESIAN_POINT ( 'NONE',  ( -9.015947181032828388E-10, -7.500000000000002665, -25.54494999981969272 ) ) ;
#6316 = AXIS2_PLACEMENT_3D ( 'NONE', #5645, #8935, #1000 ) ;
#6317 = CIRCLE ( 'NONE', #12772, 27.60000000002760245 ) ;
#6318 = CARTESIAN_POINT ( 'NONE',  ( -16.62983158437510056, 6.888301784570729502, 19.18511250018031333 ) ) ;
#6319 = DIRECTION ( 'NONE',  ( 1.000000000000000000, 0.000000000000000000, 0.000000000000000000 ) ) ;
#6320 = AXIS2_PLACEMENT_3D ( 'NONE', #16457, #14571, #17951 ) ;
#6321 = ORIENTED_EDGE ( 'NONE', *, *, #2110, .T. ) ;
#6322 = MECHANICAL_DESIGN_GEOMETRIC_PRESENTATION_REPRESENTATION (  '', ( #17505 ), #17165 ) ;
#6323 = CARTESIAN_POINT ( 'NONE',  ( -4.000000000000000000, 1.557668341133497059, -0.1596965656957516910 ) ) ;
#6324 = DIRECTION ( 'NONE',  ( -0.8191520442889896891, 1.003171929053522158E-16, 0.5735764363510490460 ) ) ;
#6325 = EDGE_LOOP ( 'NONE', ( #13791, #15376, #7809, #5299 ) ) ;
#6326 = CARTESIAN_POINT ( 'NONE',  ( -15.68987849063190687, -16.83236858365102506, -78.51413802123066432 ) ) ;
#6327 = CARTESIAN_POINT ( 'NONE',  ( 19.99999999999999645, 14.55863677812122425, 63.60407295269110506 ) ) ;
#6328 = DIRECTION ( 'NONE',  ( 1.000000000000000000, 1.836909530733573776E-16, 0.000000000000000000 ) ) ;
#6329 = CIRCLE ( 'NONE', #9721, 11.50000000000000000 ) ;
#6330 = VERTEX_POINT ( 'NONE', #7389 ) ;
#6331 = CARTESIAN_POINT ( 'NONE',  ( 3.599999999999909051, -10.82531754730554496, 43.00000000000000000 ) ) ;
#6332 = FILL_AREA_STYLE_COLOUR ( '', #20363 ) ;
#6333 = CIRCLE ( 'NONE', #13467, 0.06721999999999891950 ) ;
#6334 = CARTESIAN_POINT ( 'NONE',  ( 19.99999999999999645, 48.70996102988739551, -42.79495875147724604 ) ) ;
#6335 = CARTESIAN_POINT ( 'NONE',  ( 6.249999999999906741, -10.82531754730554496, 34.39999999999999858 ) ) ;
#6336 = CARTESIAN_POINT ( 'NONE',  ( 18.00000000043041481, 3.580422610670020322, -5.260981249819691286 ) ) ;
#6337 = VECTOR ( 'NONE', #11309, 1000.000000000000000 ) ;
#6338 = CIRCLE ( 'NONE', #18189, 2.099999999999997868 ) ;
#6339 = CARTESIAN_POINT ( 'NONE',  ( -30.00000000000000000, -124.9999999999999858, -90.00000000000001421 ) ) ;
#6340 = LINE ( 'NONE', #12502, #260 ) ;
#6341 = CARTESIAN_POINT ( 'NONE',  ( 2.943691928843430450, 14.79893867722910095, -10.78951066848092921 ) ) ;
#6342 = CARTESIAN_POINT ( 'NONE',  ( 39.99999999999999289, -122.3205080756887639, -86.97287527660684248 ) ) ;
#6343 = CIRCLE ( 'NONE', #6014, 20.00000000000000000 ) ;
#6344 = EDGE_CURVE ( 'NONE', #2456, #306, #10039, .T. ) ;
#6345 = ORIENTED_EDGE ( 'NONE', *, *, #6166, .F. ) ;
#6346 = DIRECTION ( 'NONE',  ( -1.000000000000000000, 0.000000000000000000, 0.000000000000000000 ) ) ;
#6347 = AXIS2_PLACEMENT_3D ( 'NONE', #20288, #15427, #10868 ) ;
#6348 = ADVANCED_FACE ( 'NONE', ( #18220 ), #10158, .T. ) ;
#6349 = DIRECTION ( 'NONE',  ( 0.000000000000000000, 0.000000000000000000, -1.000000000000000000 ) ) ;
#6350 = CARTESIAN_POINT ( 'NONE',  ( 150.0000507999999968, 0.000000000000000000, 0.000000000000000000 ) ) ;
#6351 = EDGE_LOOP ( 'NONE', ( #3020, #11830, #6676, #13411 ) ) ;
#6352 = DIRECTION ( 'NONE',  ( 0.000000000000000000, 0.000000000000000000, -1.000000000000000000 ) ) ;
#6353 = ORIENTED_EDGE ( 'NONE', *, *, #10920, .F. ) ;
#6354 = LINE ( 'NONE', #6659, #5802 ) ;
#6355 = LINE ( 'NONE', #14528, #2138 ) ;
#6356 = ORIENTED_EDGE ( 'NONE', *, *, #4194, .T. ) ;
#6357 = ORIENTED_EDGE ( 'NONE', *, *, #482, .T. ) ;
#6358 = DIRECTION ( 'NONE',  ( 0.000000000000000000, 0.000000000000000000, -1.000000000000000000 ) ) ;
#6359 = ADVANCED_FACE ( 'NONE', ( #12065 ), #2105, .T. ) ;
#6360 =( LENGTH_UNIT ( ) NAMED_UNIT ( * ) SI_UNIT ( .MILLI., .METRE. ) );
#6361 = CARTESIAN_POINT ( 'NONE',  ( 19.99999999999999645, 15.58726123847937828, -62.93731870009387563 ) ) ;
#6362 = CARTESIAN_POINT ( 'NONE',  ( 4.000000000000003553, -0.7779732554280839318, -0.03354435108168055818 ) ) ;
#6363 = CARTESIAN_POINT ( 'NONE',  ( -10.32494394809439875, -4.276731812588566051, -17.08395274935258001 ) ) ;
#6364 = ADVANCED_FACE ( 'NONE', ( #16726 ), #13658, .T. ) ;
#6365 = CARTESIAN_POINT ( 'NONE',  ( 4.248408730893245888, 6.358192987158590270, -19.94885624981969485 ) ) ;
#6366 = DIRECTION ( 'NONE',  ( -1.000000000000000000, 0.000000000000000000, -0.000000000000000000 ) ) ;
#6367 = CARTESIAN_POINT ( 'NONE',  ( 0.000000000000000000, -64.44931368725514176, -10.18420179740675380 ) ) ;
#6368 = DIRECTION ( 'NONE',  ( 0.000000000000000000, 0.000000000000000000, -1.000000000000000000 ) ) ;
#6369 = EDGE_CURVE ( 'NONE', #4779, #6220, #3282, .T. ) ;
#6370 = ORIENTED_EDGE ( 'NONE', *, *, #3890, .F. ) ;
#6371 = DIRECTION ( 'NONE',  ( -0.000000000000000000, -0.000000000000000000, -1.000000000000000000 ) ) ;
#6372 = EDGE_CURVE ( 'NONE', #15532, #14215, #913, .T. ) ;
#6373 = ORIENTED_EDGE ( 'NONE', *, *, #13687, .T. ) ;
#6374 = CARTESIAN_POINT ( 'NONE',  ( 3.580422614997668340, 17.99999999956958519, -18.35776874981969087 ) ) ;
#6375 = DIRECTION ( 'NONE',  ( 0.000000000000000000, 0.2697967711570248839, -0.9629172873477991335 ) ) ;
#6376 = ORIENTED_EDGE ( 'NONE', *, *, #1459, .T. ) ;
#6377 = FACE_OUTER_BOUND ( 'NONE', #8718, .T. ) ;
#6378 = ORIENTED_EDGE ( 'NONE', *, *, #9106, .F. ) ;
#6379 = DIRECTION ( 'NONE',  ( -1.000000000000000000, -0.000000000000000000, 0.000000000000000000 ) ) ;
#6380 = CARTESIAN_POINT ( 'NONE',  ( 19.99999999999999645, 0.000000000000000000, 0.000000000000000000 ) ) ;
#6381 = EDGE_CURVE ( 'NONE', #4041, #3394, #1605, .T. ) ;
#6382 = ORIENTED_EDGE ( 'NONE', *, *, #6706, .T. ) ;
#6383 = CARTESIAN_POINT ( 'NONE',  ( 6.359999999999999432, -10.85999999999998522, 1.329966423874024758E-15 ) ) ;
#6384 = DIRECTION ( 'NONE',  ( 1.000000000000000000, 0.000000000000000000, 0.000000000000000000 ) ) ;
#6385 = DIRECTION ( 'NONE',  ( -0.000000000000000000, -0.000000000000000000, 1.000000000000000000 ) ) ;
#6386 = CARTESIAN_POINT ( 'NONE',  ( 9.999999999999998224, 46.17500197033132281, -55.24372537266351912 ) ) ;
#6387 = ADVANCED_FACE ( 'NONE', ( #16932 ), #8875, .T. ) ;
#6388 = ORIENTED_EDGE ( 'NONE', *, *, #8388, .T. ) ;
#6389 = EDGE_CURVE ( 'NONE', #5687, #5684, #1370, .T. ) ;
#6390 = CARTESIAN_POINT ( 'NONE',  ( -17.50000000000000355, 2.143131898507868643E-15, 169.0000000000000000 ) ) ;
#6391 = DIRECTION ( 'NONE',  ( -0.5000000000000024425, 0.8660254037844372643, 0.000000000000000000 ) ) ;
#6392 = ORIENTED_EDGE ( 'NONE', *, *, #13835, .T. ) ;
#6393 = CARTESIAN_POINT ( 'NONE',  ( 8.899999999999895550, -10.82531754730554496, 166.0000000000000000 ) ) ;
#6394 = CARTESIAN_POINT ( 'NONE',  ( 0.000000000000000000, 0.000000000000000000, 0.000000000000000000 ) ) ;
#6395 = ORIENTED_EDGE ( 'NONE', *, *, #14772, .F. ) ;
#6396 = DIRECTION ( 'NONE',  ( 1.000000000000000000, -0.000000000000000000, -0.000000000000000000 ) ) ;
#6397 = EDGE_CURVE ( 'NONE', #14667, #17074, #11062, .T. ) ;
#6398 = CARTESIAN_POINT ( 'NONE',  ( 0.000000000000000000, 0.000000000000000000, 0.000000000000000000 ) ) ;
#6399 = DIRECTION ( 'NONE',  ( -1.000000000000000000, 0.000000000000000000, 0.000000000000000000 ) ) ;
#6400 = ORIENTED_EDGE ( 'NONE', *, *, #2403, .T. ) ;
#6401 = DIRECTION ( 'NONE',  ( 1.000000000000000000, 0.000000000000000000, 0.000000000000000000 ) ) ;
#6402 = ORIENTED_EDGE ( 'NONE', *, *, #5658, .F. ) ;
#6403 = DIRECTION ( 'NONE',  ( 0.000000000000000000, 0.000000000000000000, 1.000000000000000000 ) ) ;
#6404 = ORIENTED_EDGE ( 'NONE', *, *, #6822, .F. ) ;
#6405 = DIRECTION ( 'NONE',  ( -1.000000000000000000, 0.000000000000000000, -0.000000000000000000 ) ) ;
#6406 = CARTESIAN_POINT ( 'NONE',  ( 19.99999999999999645, 6.872116855664026858, -64.47358224882410127 ) ) ;
#6407 = CARTESIAN_POINT ( 'NONE',  ( 14.79893867758297610, -1.779016607511492805E-09, -12.53470808115845969 ) ) ;
#6408 = ORIENTED_EDGE ( 'NONE', *, *, #15947, .F. ) ;
#6409 = CARTESIAN_POINT ( 'NONE',  ( 19.99999999999999645, -27.80658314415179078, -66.41380830714150818 ) ) ;
#6410 = DIRECTION ( 'NONE',  ( 1.000000000000000000, 0.000000000000000000, 0.000000000000000000 ) ) ;
#6411 = ORIENTED_EDGE ( 'NONE', *, *, #13134, .F. ) ;
#6412 = CARTESIAN_POINT ( 'NONE',  ( 6.991428239010133439, -20.34384952674291469, 76.59572168033703576 ) ) ;
#6413 = CYLINDRICAL_SURFACE ( 'NONE', #18316, 20.00000000000000000 ) ;
#6414 = FACE_OUTER_BOUND ( 'NONE', #5153, .T. ) ;
#6415 = CARTESIAN_POINT ( 'NONE',  ( 2.500000000000000000, 2.357898499370431722, -2.818925648462311528E-15 ) ) ;
#6416 = AXIS2_PLACEMENT_3D ( 'NONE', #8015, #11097, #7593 ) ;
#6417 = EDGE_LOOP ( 'NONE', ( #19331, #2057, #16028, #4385 ) ) ;
#6418 = DIRECTION ( 'NONE',  ( 1.000000000000000000, 0.000000000000000000, 0.000000000000000000 ) ) ;
#6419 = CARTESIAN_POINT ( 'NONE',  ( 19.99999999999999645, 0.000000000000000000, 0.000000000000000000 ) ) ;
#6420 = ORIENTED_EDGE ( 'NONE', *, *, #14076, .F. ) ;
#6421 = DIRECTION ( 'NONE',  ( -1.000000000000000000, 0.000000000000000000, 0.000000000000000000 ) ) ;
#6422 = FACE_OUTER_BOUND ( 'NONE', #15793, .T. ) ;
#6423 = DIRECTION ( 'NONE',  ( 0.000000000000000000, 0.000000000000000000, 1.000000000000000000 ) ) ;
#6424 = EDGE_CURVE ( 'NONE', #2180, #14573, #6317, .T. ) ;
#6425 = VERTEX_POINT ( 'NONE', #9099 ) ;
#6426 = DIRECTION ( 'NONE',  ( 0.000000000000000000, -1.000000000000000000, 0.000000000000000000 ) ) ;
#6427 = DIRECTION ( 'NONE',  ( 0.000000000000000000, -0.5195839500354404450, 0.8544194045464844622 ) ) ;
#6428 = CARTESIAN_POINT ( 'NONE',  ( 0.000000000000000000, -63.85430960833482317, 16.34407078397855528 ) ) ;
#6429 = DIRECTION ( 'NONE',  ( -0.1301338387963445475, -0.9914964367057137462, 1.131240564625405124E-16 ) ) ;
#6430 = CARTESIAN_POINT ( 'NONE',  ( 12.72792206288791128, 12.72792205982780267, -15.56957499981969484 ) ) ;
#6431 = ORIENTED_EDGE ( 'NONE', *, *, #15767, .F. ) ;
#6432 = CARTESIAN_POINT ( 'NONE',  ( -24.99999999999999289, -85.00000000000000000, -1.040949779275250179E-14 ) ) ;
#6433 = CARTESIAN_POINT ( 'NONE',  ( 8.899999999999895550, -10.82531754730554496, 43.00000000000000000 ) ) ;
#6434 = CARTESIAN_POINT ( 'NONE',  ( -14.79893867722910095, 2.943691928843434891, -13.14576066848092673 ) ) ;
#6435 = CYLINDRICAL_SURFACE ( 'NONE', #16670, 10.52399999999999558 ) ;
#6436 = VECTOR ( 'NONE', #16562, 1000.000000000000000 ) ;
#6437 = ORIENTED_EDGE ( 'NONE', *, *, #3653, .T. ) ;
#6438 = DIRECTION ( 'NONE',  ( 0.000000000000000000, 0.000000000000000000, 1.000000000000000000 ) ) ;
#6439 = CARTESIAN_POINT ( 'NONE',  ( -6.358192987158597376, 4.248408730893249441, 21.65979375018031661 ) ) ;
#6440 = CARTESIAN_POINT ( 'NONE',  ( 6.250000000000054179, 10.82531754730546147, 43.00000000000000000 ) ) ;
#6441 = EDGE_LOOP ( 'NONE', ( #20606, #19757, #14209, #9585 ) ) ;
#6442 = CARTESIAN_POINT ( 'NONE',  ( 19.99999999999999645, 23.08379033237438094, -61.02926039941409897 ) ) ;
#6443 = ORIENTED_EDGE ( 'NONE', *, *, #7260, .F. ) ;
#6444 = DIRECTION ( 'NONE',  ( 1.000000000000000000, 0.000000000000000000, 0.000000000000000000 ) ) ;
#6445 = CARTESIAN_POINT ( 'NONE',  ( 3.580422614997667896, 17.99999999956958163, 19.34223125018031197 ) ) ;
#6446 = EDGE_CURVE ( 'NONE', #18079, #17770, #6022, .T. ) ;
#6447 = VECTOR ( 'NONE', #10326, 1000.000000000000000 ) ;
#6448 = ORIENTED_EDGE ( 'NONE', *, *, #17544, .T. ) ;
#6449 = ORIENTED_EDGE ( 'NONE', *, *, #8651, .T. ) ;
#6450 = CARTESIAN_POINT ( 'NONE',  ( 49.19234958605026264, -1.326995226329880762, -84.99999999999998579 ) ) ;
#6451 = VECTOR ( 'NONE', #6153, 1000.000000000000000 ) ;
#6452 = VECTOR ( 'NONE', #2361, 1000.000000000000000 ) ;
#6453 =( NAMED_UNIT ( * ) SI_UNIT ( $, .STERADIAN. ) SOLID_ANGLE_UNIT ( ) );
#6454 = DIRECTION ( 'NONE',  ( 1.000000000000000000, 0.000000000000000000, 0.000000000000000000 ) ) ;
#6455 = EDGE_CURVE ( 'NONE', #9717, #4014, #1272, .T. ) ;
#6456 = DIRECTION ( 'NONE',  ( -1.000000000000000000, -0.000000000000000000, 0.000000000000000000 ) ) ;
#6457 = CARTESIAN_POINT ( 'NONE',  ( 5.303300858261588147, -5.303300859536636658, 17.24182500018031661 ) ) ;
#6458 = CARTESIAN_POINT ( 'NONE',  ( 10.32494394809438987, 4.276731812588564274, -0.6441722502868038047 ) ) ;
#6459 = CARTESIAN_POINT ( 'NONE',  ( 0.000000000000000000, -27.80658314415272514, 66.41380830714115291 ) ) ;
#6460 = DIRECTION ( 'NONE',  ( -1.000000000000000000, -0.000000000000000000, -0.000000000000000000 ) ) ;
#6461 = DIRECTION ( 'NONE',  ( -0.000000000000000000, -0.000000000000000000, 1.000000000000000000 ) ) ;
#6462 = ORIENTED_EDGE ( 'NONE', *, *, #10399, .F. ) ;
#6463 = CARTESIAN_POINT ( 'NONE',  ( 0.000000000000000000, 54.08351995568706627, 35.76369202524519864 ) ) ;
#6464 = ORIENTED_EDGE ( 'NONE', *, *, #8501, .T. ) ;
#6465 = CARTESIAN_POINT ( 'NONE',  ( 17.99999999956958163, -3.580422614997676334, 14.17808125018031440 ) ) ;
#6466 = CARTESIAN_POINT ( 'NONE',  ( -30.00000000000000000, -164.9999999999999716, -50.00000000000000711 ) ) ;
#6467 = AXIS2_PLACEMENT_3D ( 'NONE', #5400, #855, #20017 ) ;
#6468 = EDGE_LOOP ( 'NONE', ( #11111, #16484, #4913, #3071 ) ) ;
#6469 = CARTESIAN_POINT ( 'NONE',  ( 0.2500000000000002220, 0.000000000000000000, 0.000000000000000000 ) ) ;
#6470 = EDGE_LOOP ( 'NONE', ( #10872, #11075, #10292, #10874 ) ) ;
#6471 = DIRECTION ( 'NONE',  ( 0.000000000000000000, 0.000000000000000000, 1.000000000000000000 ) ) ;
#6472 = CARTESIAN_POINT ( 'NONE',  ( -7.500000000000002665, -4.022542205827308438E-17, 14.51130000000230602 ) ) ;
#6473 = ORIENTED_EDGE ( 'NONE', *, *, #12086, .F. ) ;
#6474 = VERTEX_POINT ( 'NONE', #20736 ) ;
#6475 = LINE ( 'NONE', #11470, #11042 ) ;
#6476 = DIRECTION ( 'NONE',  ( 1.000000000000000000, 0.000000000000000000, 0.000000000000000000 ) ) ;
#6477 = AXIS2_PLACEMENT_3D ( 'NONE', #951, #5481, #12166 ) ;
#6478 = EDGE_CURVE ( 'NONE', #9154, #1772, #15803, .T. ) ;
#6479 = EDGE_CURVE ( 'NONE', #19715, #12410, #18954, .T. ) ;
#6480 = CARTESIAN_POINT ( 'NONE',  ( 19.99999999999999645, -59.31169354540720207, -27.19476070466916795 ) ) ;
#6481 = AXIS2_PLACEMENT_3D ( 'NONE', #4974, #19590, #5064 ) ;
#6482 = ORIENTED_EDGE ( 'NONE', *, *, #5221, .T. ) ;
#6483 = CARTESIAN_POINT ( 'NONE',  ( -6.929096493489625530, 2.870125743571138255, 15.10036250018031367 ) ) ;
#6484 = EDGE_CURVE ( 'NONE', #9398, #18276, #9512, .T. ) ;
#6485 = CARTESIAN_POINT ( 'NONE',  ( -1.491842756249033286, -7.499999999820668783, -0.1355187498196866458 ) ) ;
#6486 = EDGE_CURVE ( 'NONE', #5273, #20260, #5310, .T. ) ;
#6487 = MECHANICAL_DESIGN_GEOMETRIC_PRESENTATION_REPRESENTATION (  '', ( #12939 ), #68 ) ;
#6488 = DIRECTION ( 'NONE',  ( 1.000000000000000000, -0.000000000000000000, -0.000000000000000000 ) ) ;
#6489 = CARTESIAN_POINT ( 'NONE',  ( 0.000000000000000000, 64.52323195238639642, -6.389157729492497495 ) ) ;
#6490 = EDGE_LOOP ( 'NONE', ( #4366, #2498, #2276, #6529 ) ) ;
#6491 = CARTESIAN_POINT ( 'NONE',  ( 0.000000000000000000, -55.05624179291956466, -35.01774179823839717 ) ) ;
#6492 = CARTESIAN_POINT ( 'NONE',  ( -15.25966316918061771, 10.19618095414378622, 17.57504375018031695 ) ) ;
#6493 = DIRECTION ( 'NONE',  ( 0.000000000000000000, 0.1361666490962468723, -0.9906859460363307557 ) ) ;
#6494 = VECTOR ( 'NONE', #7893, 1000.000000000000000 ) ;
#6495 = ORIENTED_EDGE ( 'NONE', *, *, #10802, .F. ) ;
#6496 = AXIS2_PLACEMENT_3D ( 'NONE', #13472, #6880, #18022 ) ;
#6497 = CARTESIAN_POINT ( 'NONE',  ( 0.000000000000000000, 0.000000000000000000, 40.00000000000000000 ) ) ;
#6498 = ORIENTED_EDGE ( 'NONE', *, *, #18557, .T. ) ;
#6499 = DIRECTION ( 'NONE',  ( -1.000000000000000000, -0.000000000000000000, 0.000000000000000000 ) ) ;
#6500 = AXIS2_PLACEMENT_3D ( 'NONE', #2433, #7306, #15371 ) ;
#6501 = ORIENTED_EDGE ( 'NONE', *, *, #4654, .T. ) ;
#6502 = EDGE_CURVE ( 'NONE', #1227, #15433, #17175, .T. ) ;
#6503 = CARTESIAN_POINT ( 'NONE',  ( 38.52090548607635867, -121.4001261175067299, 79.56756026429930273 ) ) ;
#6504 = EDGE_CURVE ( 'NONE', #20567, #19615, #14143, .T. ) ;
#6505 = DIRECTION ( 'NONE',  ( 0.000000000000000000, 0.000000000000000000, -1.000000000000000000 ) ) ;
#6506 = CARTESIAN_POINT ( 'NONE',  ( 11.17563879731705789, -1.343450868547281933E-09, 25.91760975064743278 ) ) ;
#6507 = VECTOR ( 'NONE', #5918, 1000.000000000000000 ) ;
#6509 = VERTEX_POINT ( 'NONE', #14195 ) ;
#6508 = CIRCLE ( 'NONE', #5488, 10.52399999999999558 ) ;
#6511 = ADVANCED_FACE ( 'NONE', ( #13976 ), #18748, .T. ) ;
#6510 = DIRECTION ( 'NONE',  ( 1.000000000000000000, 0.000000000000000000, 0.000000000000000000 ) ) ;
#6512 = CARTESIAN_POINT ( 'NONE',  ( 0.000000000000000000, 51.96384592647199696, 49.83732252579633126 ) ) ;
#6513 = AXIS2_PLACEMENT_3D ( 'NONE', #8352, #18000, #5164 ) ;
#6514 = ORIENTED_EDGE ( 'NONE', *, *, #4005, .T. ) ;
#6515 = FACE_OUTER_BOUND ( 'NONE', #946, .T. ) ;
#6516 = CARTESIAN_POINT ( 'NONE',  ( -10.19618095414378622, -15.25966316918061416, 17.12339375018031262 ) ) ;
#6517 = DIRECTION ( 'NONE',  ( -1.000000000000000000, 0.000000000000000000, 0.000000000000000000 ) ) ;
#6518 = CARTESIAN_POINT ( 'NONE',  ( 0.000000000000000000, 0.000000000000000000, -5.574599999999999334 ) ) ;
#6519 = CIRCLE ( 'NONE', #6176, 2.649999999999993694 ) ;
#6520 = VERTEX_POINT ( 'NONE', #5914 ) ;
#6521 = DIRECTION ( 'NONE',  ( 1.000000000000000000, 0.000000000000000000, 0.000000000000000000 ) ) ;
#6522 = ORIENTED_EDGE ( 'NONE', *, *, #3897, .T. ) ;
#6523 = CIRCLE ( 'NONE', #7184, 4.000000000000000000 ) ;
#6524 = DIRECTION ( 'NONE',  ( -0.000000000000000000, -0.000000000000000000, 1.000000000000000000 ) ) ;
#6525 = CIRCLE ( 'NONE', #18378, 11.50000000000000000 ) ;
#6526 = EDGE_CURVE ( 'NONE', #2254, #15842, #6661, .T. ) ;
#6527 = LINE ( 'NONE', #13012, #9683 ) ;
#6528 = CARTESIAN_POINT ( 'NONE',  ( 9.015937996181842420E-10, 7.500000000000007994, -5.142549999819685524 ) ) ;
#6529 = ORIENTED_EDGE ( 'NONE', *, *, #14962, .T. ) ;
#6530 = CARTESIAN_POINT ( 'NONE',  ( 19.99999999999999645, 64.52323195238639642, -6.389157729492497495 ) ) ;
#6531 = CARTESIAN_POINT ( 'NONE',  ( 19.99999999999999645, 36.59093685910629290, 62.00889726308042782 ) ) ;
#6532 =( LENGTH_UNIT ( ) NAMED_UNIT ( * ) SI_UNIT ( .MILLI., .METRE. ) );
#6533 = VECTOR ( 'NONE', #19085, 999.9999999999997726 ) ;
#6534 = CARTESIAN_POINT ( 'NONE',  ( -6.888301780572502864, 16.62983158603122646, -17.33676249981969164 ) ) ;
#6535 = AXIS2_PLACEMENT_3D ( 'NONE', #5308, #5405, #10186 ) ;
#6536 = ORIENTED_EDGE ( 'NONE', *, *, #17056, .T. ) ;
#6537 = CARTESIAN_POINT ( 'NONE',  ( 19.99999999999999645, 55.05624179291979914, 35.01774179823801347 ) ) ;
#6538 = VECTOR ( 'NONE', #14784, 1000.000000000000000 ) ;
#6539 = LINE ( 'NONE', #17990, #14165 ) ;
#6540 = CIRCLE ( 'NONE', #18396, 27.60000000002759890 ) ;
#6541 = CARTESIAN_POINT ( 'NONE',  ( -8.382925368423267187, 12.54593441764186856, -2.542635668480925037 ) ) ;
#6542 = ADVANCED_FACE ( 'NONE', ( #10797 ), #17258, .T. ) ;
#6543 = DIRECTION ( 'NONE',  ( 1.000000000000000000, 1.836909530733573776E-16, 0.000000000000000000 ) ) ;
#6544 = ORIENTED_EDGE ( 'NONE', *, *, #10240, .F. ) ;
#6545 = CYLINDRICAL_SURFACE ( 'NONE', #9578, 27.60000000002760245 ) ;
#6546 = CYLINDRICAL_SURFACE ( 'NONE', #19539, 65.24900000006525147 ) ;
#6547 = CIRCLE ( 'NONE', #20777, 2.649999999999994582 ) ;
#6548 = ORIENTED_EDGE ( 'NONE', *, *, #1722, .F. ) ;
#6549 = AXIS2_PLACEMENT_3D ( 'NONE', #12281, #1279, #9517 ) ;
#6550 = CARTESIAN_POINT ( 'NONE',  ( -62.49999999999999289, -120.0000000000000142, 5.000000000000000000 ) ) ;
#6551 = ORIENTED_EDGE ( 'NONE', *, *, #5221, .F. ) ;
#6552 = CARTESIAN_POINT ( 'NONE',  ( 24.99999999999999645, -85.00000000000000000, -1.040949779275250179E-14 ) ) ;
#6553 = CARTESIAN_POINT ( 'NONE',  ( -18.00000000043040771, -3.580422610670021211, 16.39691875018030842 ) ) ;
#6554 = EDGE_LOOP ( 'NONE', ( #7550, #7063, #20786, #5857 ) ) ;
#6555 = ORIENTED_EDGE ( 'NONE', *, *, #10108, .T. ) ;
#6556 = CARTESIAN_POINT ( 'NONE',  ( -24.99999999999999289, 230.0000000000000000, 85.00000000000000000 ) ) ;
#6557 = AXIS2_PLACEMENT_3D ( 'NONE', #893, #20271, #17106 ) ;
#6558 = CIRCLE ( 'NONE', #16061, 2.055000000000000160 ) ;
#6559 = DIRECTION ( 'NONE',  ( 1.000000000000000000, 0.000000000000000000, 0.000000000000000000 ) ) ;
#6560 =( NAMED_UNIT ( * ) SI_UNIT ( $, .STERADIAN. ) SOLID_ANGLE_UNIT ( ) );
#6561 = CARTESIAN_POINT ( 'NONE',  ( 2.500000000000000000, 1.178949249685213863, -2.042000000000001148 ) ) ;
#6562 = DIRECTION ( 'NONE',  ( -6.938893903907228378E-17, 1.000000000000000000, -0.000000000000000000 ) ) ;
#6563 = CARTESIAN_POINT ( 'NONE',  ( 6.358192988180019434, 4.248408729364581582, 15.18010625018031590 ) ) ;
#6564 = VECTOR ( 'NONE', #16676, 1000.000000000000000 ) ;
#6565 = CARTESIAN_POINT ( 'NONE',  ( -7.902369976724391343, 7.902369978624323110, 5.835515249713198571 ) ) ;
#6566 = EDGE_CURVE ( 'NONE', #1433, #18811, #17402, .T. ) ;
#6567 = CIRCLE ( 'NONE', #1181, 65.24900000006525147 ) ;
#6568 = LINE ( 'NONE', #11544, #10464 ) ;
#6569 = DIRECTION ( 'NONE',  ( 0.000000000000000000, 0.000000000000000000, 1.000000000000000000 ) ) ;
#6570 = AXIS2_PLACEMENT_3D ( 'NONE', #11359, #17833, #3306 ) ;
#6571 = ORIENTED_EDGE ( 'NONE', *, *, #3510, .F. ) ;
#6572 = FACE_OUTER_BOUND ( 'NONE', #11665, .T. ) ;
#6573 = CARTESIAN_POINT ( 'NONE',  ( 10.19618095414378800, 15.25966316918061416, 21.83589375018031831 ) ) ;
#6574 = LINE ( 'NONE', #4781, #8598 ) ;
#6575 = VERTEX_POINT ( 'NONE', #1773 ) ;
#6576 = DIRECTION ( 'NONE',  ( -0.000000000000000000, -0.000000000000000000, 1.000000000000000000 ) ) ;
#6577 = VERTEX_POINT ( 'NONE', #19467 ) ;
#6578 = CARTESIAN_POINT ( 'NONE',  ( -31.74999999999995737, 0.000000000000000000, 0.000000000000000000 ) ) ;
#6579 = CARTESIAN_POINT ( 'NONE',  ( 30.88247860994248128, -39.30399960665665304, -66.45597419381263649 ) ) ;
#6580 = VERTEX_POINT ( 'NONE', #19663 ) ;
#6581 = ORIENTED_EDGE ( 'NONE', *, *, #10428, .T. ) ;
#6582 = CARTESIAN_POINT ( 'NONE',  ( 19.99999999999999645, -42.42902769288503606, -49.02903636734241388 ) ) ;
#6583 = CARTESIAN_POINT ( 'NONE',  ( 2.000000000000010658, -3.464101615137748169, 0.000000000000000000 ) ) ;
#6584 = AXIS2_PLACEMENT_3D ( 'NONE', #4724, #17768, #16174 ) ;
#6585 = CARTESIAN_POINT ( 'NONE',  ( 6.232799999999996565, 0.000000000000000000, 0.000000000000000000 ) ) ;
#6586 = ORIENTED_EDGE ( 'NONE', *, *, #6989, .F. ) ;
#6587 = CARTESIAN_POINT ( 'NONE',  ( 5.303300859536630441, 5.303300858261584594, 8.620675000180311187 ) ) ;
#6588 = DIRECTION ( 'NONE',  ( -0.000000000000000000, -0.000000000000000000, -1.000000000000000000 ) ) ;
#6589 = CARTESIAN_POINT ( 'NONE',  ( 9.999999999999998224, -68.15657073222450890, 23.20952102120258331 ) ) ;
#6590 = CARTESIAN_POINT ( 'NONE',  ( 19.99999999999999645, 0.000000000000000000, 0.000000000000000000 ) ) ;
#6591 = CARTESIAN_POINT ( 'NONE',  ( 1.040949779275250179E-14, -85.00000000000000000, 19.00000000000000000 ) ) ;
#6592 = ORIENTED_EDGE ( 'NONE', *, *, #20613, .T. ) ;
#6593 = DIRECTION ( 'NONE',  ( -1.000000000000000000, -0.000000000000000000, 0.000000000000000000 ) ) ;
#6594 = ORIENTED_EDGE ( 'NONE', *, *, #13605, .F. ) ;
#6595 = CARTESIAN_POINT ( 'NONE',  ( -18.00000000000000000, 2.163826221265758884E-09, 16.69145000018031411 ) ) ;
#6596 = LINE ( 'NONE', #8297, #13008 ) ;
#6597 = EDGE_LOOP ( 'NONE', ( #7651, #14778 ) ) ;
#6598 = EDGE_CURVE ( 'NONE', #10440, #15031, #9725, .T. ) ;
#6599 = DIRECTION ( 'NONE',  ( 0.000000000000000000, 0.000000000000000000, 1.000000000000000000 ) ) ;
#6600 = VERTEX_POINT ( 'NONE', #12817 ) ;
#6601 = VECTOR ( 'NONE', #1330, 1000.000000000000000 ) ;
#6602 = DIRECTION ( 'NONE',  ( -0.000000000000000000, -0.000000000000000000, 1.000000000000000000 ) ) ;
#6603 = ADVANCED_FACE ( 'NONE', ( #16193 ), #3355, .T. ) ;
#6604 = EDGE_LOOP ( 'NONE', ( #15534, #12368, #19118, #4759, #2555, #6988, #8450 ) ) ;
#6605 = ADVANCED_FACE ( 'NONE', ( #19570 ), #237, .F. ) ;
#6606 = DIRECTION ( 'NONE',  ( -1.000000000000000000, 0.000000000000000000, -0.000000000000000000 ) ) ;
#6607 = VECTOR ( 'NONE', #1321, 1000.000000000000000 ) ;
#6608 = CARTESIAN_POINT ( 'NONE',  ( 7.000000000000000888, -10.52399999999998670, 1.288818291422673781E-15 ) ) ;
#6609 = CARTESIAN_POINT ( 'NONE',  ( 6.330490858644141738, 9.474249097082498849, 24.44495350064742922 ) ) ;
#6610 = ORIENTED_EDGE ( 'NONE', *, *, #6254, .F. ) ;
#6611 = DIRECTION ( 'NONE',  ( 0.000000000000000000, -1.000000000000000000, 0.000000000000000000 ) ) ;
#6612 = CARTESIAN_POINT ( 'NONE',  ( 0.000000000000000000, 0.000000000000000000, 0.000000000000000000 ) ) ;
#6613 = ORIENTED_EDGE ( 'NONE', *, *, #19718, .T. ) ;
#6614 = CARTESIAN_POINT ( 'NONE',  ( -20.80121494421295125, -5.547499958777468265, -80.68520720011532887 ) ) ;
#6615 = EDGE_CURVE ( 'NONE', #14502, #17420, #13785, .T. ) ;
#6616 = DIRECTION ( 'NONE',  ( 0.000000000000000000, 0.000000000000000000, 1.000000000000000000 ) ) ;
#6617 = DIRECTION ( 'NONE',  ( -0.7071067811865364705, 8.659560562355067211E-17, -0.7071067811865584529 ) ) ;
#6618 = FACE_OUTER_BOUND ( 'NONE', #8087, .T. ) ;
#6619 = EDGE_CURVE ( 'NONE', #5352, #2775, #1929, .T. ) ;
#6620 = AXIS2_PLACEMENT_3D ( 'NONE', #17687, #1480, #19064 ) ;
#6621 = EDGE_LOOP ( 'NONE', ( #14914, #14976, #20483, #6798, #14427, #18165, #15575, #8711, #2382 ) ) ;
#6622 = CIRCLE ( 'NONE', #9016, 75.00000000000001421 ) ;
#6623 = ADVANCED_FACE ( 'NONE', ( #11509 ), #6734, .F. ) ;
#6624 = CARTESIAN_POINT ( 'NONE',  ( -4.000000000000000000, 0.3904826640788011116, -3.430483436379915141E-17 ) ) ;
#6625 = VERTEX_POINT ( 'NONE', #18092 ) ;
#6626 = FACE_OUTER_BOUND ( 'NONE', #20409, .T. ) ;
#6627 = CIRCLE ( 'NONE', #15098, 17.50000000000000355 ) ;
#6628 = CIRCLE ( 'NONE', #16787, 23.00000000000000000 ) ;
#6629 = DIRECTION ( 'NONE',  ( -1.000000000000000000, -0.000000000000000000, 0.000000000000000000 ) ) ;
#6630 = FACE_OUTER_BOUND ( 'NONE', #20266, .T. ) ;
#6631 = ADVANCED_FACE ( 'NONE', ( #14510 ), #19361, .T. ) ;
#6632 = EDGE_LOOP ( 'NONE', ( #87, #11751, #1841, #4353 ) ) ;
#6633 = DIRECTION ( 'NONE',  ( -1.000000000000000000, 0.000000000000000000, -0.000000000000000000 ) ) ;
#6634 = AXIS2_PLACEMENT_3D ( 'NONE', #3204, #1922, #13058 ) ;
#6635 = DIRECTION ( 'NONE',  ( 0.000000000000000000, 0.000000000000000000, -1.000000000000000000 ) ) ;
#6636 = DIRECTION ( 'NONE',  ( -0.1301338387963444088, -0.9914964367057135242, 1.243481486083094649E-31 ) ) ;
#6637 = CARTESIAN_POINT ( 'NONE',  ( -15.25966317163203456, -10.19618095047498230, -19.98754374981969661 ) ) ;
#6638 = ORIENTED_EDGE ( 'NONE', *, *, #3058, .T. ) ;
#6639 = AXIS2_PLACEMENT_3D ( 'NONE', #6862, #3290, #8257 ) ;
#6640 = CIRCLE ( 'NONE', #14111, 0.2000000000000000944 ) ;
#6641 = CARTESIAN_POINT ( 'NONE',  ( 17.00000000000000000, 0.000000000000000000, 0.000000000000000000 ) ) ;
#6642 = CARTESIAN_POINT ( 'NONE',  ( 19.99999999999999645, 0.000000000000000000, 0.000000000000000000 ) ) ;
#6643 = EDGE_CURVE ( 'NONE', #17243, #16003, #3297, .T. ) ;
#6644 = VECTOR ( 'NONE', #11438, 1000.000000000000000 ) ;
#6645 = CIRCLE ( 'NONE', #18508, 10.52399999999999558 ) ;
#6646 = CARTESIAN_POINT ( 'NONE',  ( 14.79893867793683349, 2.943691925285396582, -9.022323168480927080 ) ) ;
#6647 = EDGE_CURVE ( 'NONE', #12774, #5100, #3613, .T. ) ;
#6648 = PRESENTATION_LAYER_ASSIGNMENT (  '', '', ( #1610 ) ) ;
#6649 = FACE_OUTER_BOUND ( 'NONE', #20796, .T. ) ;
#6650 = ORIENTED_EDGE ( 'NONE', *, *, #962, .F. ) ;
#6651 = FACE_OUTER_BOUND ( 'NONE', #20921, .T. ) ;
#6652 = EDGE_CURVE ( 'NONE', #7841, #5402, #4976, .T. ) ;
#6653 = AXIS2_PLACEMENT_3D ( 'NONE', #15820, #1319, #9253 ) ;
#6654 = CARTESIAN_POINT ( 'NONE',  ( -30.00000000000000000, -49.99999999999999289, -71.93747284969079203 ) ) ;
#6655 = FACE_OUTER_BOUND ( 'NONE', #14318, .T. ) ;
#6656 = ORIENTED_EDGE ( 'NONE', *, *, #12214, .T. ) ;
#6657 = DIRECTION ( 'NONE',  ( -1.000000000000000000, 0.000000000000000000, 0.000000000000000000 ) ) ;
#6658 = VERTEX_POINT ( 'NONE', #6331 ) ;
#6659 = CARTESIAN_POINT ( 'NONE',  ( 19.99999999999999645, -64.80702306891100761, 7.581672767546201008 ) ) ;
#6660 = DIRECTION ( 'NONE',  ( 0.000000000000000000, 0.2697967711570248839, -0.9629172873477991335 ) ) ;
#6661 = CIRCLE ( 'NONE', #924, 11.49999999999999467 ) ;
#6662 = ORIENTED_EDGE ( 'NONE', *, *, #5070, .T. ) ;
#6663 = ORIENTED_EDGE ( 'NONE', *, *, #16497, .T. ) ;
#6664 = CARTESIAN_POINT ( 'NONE',  ( 49.01761906262722590, -1.923047794321506743, -84.32426567686945873 ) ) ;
#6665 = VECTOR ( 'NONE', #12583, 1000.000000000000000 ) ;
#6666 = AXIS2_PLACEMENT_3D ( 'NONE', #10167, #5703, #7080 ) ;
#6667 = FACE_OUTER_BOUND ( 'NONE', #9037, .T. ) ;
#6668 = DIRECTION ( 'NONE',  ( 0.000000000000000000, 0.000000000000000000, -1.000000000000000000 ) ) ;
#6669 = CARTESIAN_POINT ( 'NONE',  ( -1.491842754445842800, 7.500000000179346316, 22.83791875018031803 ) ) ;
#6670 = CARTESIAN_POINT ( 'NONE',  ( 10.32494394809438987, 4.276731812588564274, 8.780827749713202124 ) ) ;
#6671 = CIRCLE ( 'NONE', #15488, 17.50000000000000355 ) ;
#6672 =( BOUNDED_CURVE ( )  B_SPLINE_CURVE ( 2, ( #18908, #1212, #19002, #2684, #14349, #14034, #6277, #11054, #7765, #12764, #5960, #9559, #4589, #14236, #1528, #18797, #19215 ),
 .UNSPECIFIED., .F., .T. ) 
 B_SPLINE_CURVE_WITH_KNOTS ( ( 3, 2, 2, 2, 2, 2, 2, 2, 3 ),
 ( 0.4000000000038512193, 0.4125000000038511749, 0.4250000000038511860, 0.4375000000038511971, 0.4500000000038512082, 0.4625000000038511638, 0.4750000000038511194, 0.4875000000038511305, 0.5000000000038511416 ),
 .UNSPECIFIED. ) 
 CURVE ( )  GEOMETRIC_REPRESENTATION_ITEM ( )  RATIONAL_B_SPLINE_CURVE ( ( 0.9999999999940800688, 0.9807852804091503618, 1.000000000000000000, 0.9807852804032304306, 1.000000000000000000, 0.9807852804032304306, 1.000000000000000000, 0.9807852804032304306, 1.000000000000000000, 0.9807852804032304306, 1.000000000000000000, 0.9807852804032304306, 1.000000000000000000, 0.9807852804032304306, 1.000000000000000000, 0.9807852803973104994, 1.000000000005919931 ) ) 
 REPRESENTATION_ITEM ( '' )  );
#6673 = DIRECTION ( 'NONE',  ( -1.000000000000000000, 0.000000000000000000, 0.000000000000000000 ) ) ;
#6674 = CARTESIAN_POINT ( 'NONE',  ( -22.96694501150314238, -24.74873734152930993, -120.0000000000000142 ) ) ;
#6675 = CIRCLE ( 'NONE', #1621, 72.00000000007199219 ) ;
#6676 = ORIENTED_EDGE ( 'NONE', *, *, #3985, .T. ) ;
#6677 = AXIS2_PLACEMENT_3D ( 'NONE', #4289, #3962, #18496 ) ;
#6678 = CARTESIAN_POINT ( 'NONE',  ( 6.250000000000054179, 10.82531754730546147, 46.00000000000000711 ) ) ;
#6679 = CARTESIAN_POINT ( 'NONE',  ( 17.99999999956958163, -3.580422614997676334, -25.42651874981968874 ) ) ;
#6680 = CARTESIAN_POINT ( 'NONE',  ( 0.000000000000000000, 0.000000000000000000, 0.000000000000000000 ) ) ;
#6681 = ORIENTED_EDGE ( 'NONE', *, *, #15852, .T. ) ;
#6682 = FACE_OUTER_BOUND ( 'NONE', #14526, .T. ) ;
#6683 = ORIENTED_EDGE ( 'NONE', *, *, #4027, .F. ) ;
#6684 = DIRECTION ( 'NONE',  ( 0.000000000000000000, -0.8169698930104470902, 0.5766803221148600889 ) ) ;
#6685 = CARTESIAN_POINT ( 'NONE',  ( 38.31677532819030318, -18.47596261708826049, 77.53674502934073587 ) ) ;
#6686 = ORIENTED_EDGE ( 'NONE', *, *, #10468, .T. ) ;
#6687 =( REPRESENTATION_RELATIONSHIP ('NONE','NONE', #13739, #2344 ) REPRESENTATION_RELATIONSHIP_WITH_TRANSFORMATION ( #13952 )SHAPE_REPRESENTATION_RELATIONSHIP( ) );
#6688 = EDGE_LOOP ( 'NONE', ( #20302, #6002, #13742 ) ) ;
#6689 = DIRECTION ( 'NONE',  ( -0.000000000000000000, -0.000000000000000000, 1.000000000000000000 ) ) ;
#6690 = EDGE_CURVE ( 'NONE', #19935, #10395, #15137, .T. ) ;
#6691 = ADVANCED_FACE ( 'NONE', ( #17682, #9723 ), #3153, .F. ) ;
#6692 = SURFACE_SIDE_STYLE ('',( #13170 ) ) ;
#6693 = CARTESIAN_POINT ( 'NONE',  ( 0.000000000000000000, 46.17500197033132991, -55.24372537266351912 ) ) ;
#6694 = CARTESIAN_POINT ( 'NONE',  ( 30.00000000000000000, -39.99999999999999289, -49.89999999999999858 ) ) ;
#6695 = ORIENTED_EDGE ( 'NONE', *, *, #1090, .F. ) ;
#6696 = CARTESIAN_POINT ( 'NONE',  ( 19.99999999999999645, 71.76067541710850151, 5.865617076724869428 ) ) ;
#6697 = CARTESIAN_POINT ( 'NONE',  ( -6.232800000000000118, 0.000000000000000000, 0.000000000000000000 ) ) ;
#6698 = CARTESIAN_POINT ( 'NONE',  ( 0.000000000000000000, 45.48683723007212620, 46.78012013466234720 ) ) ;
#6699 = FACE_OUTER_BOUND ( 'NONE', #5877, .T. ) ;
#6700 = CARTESIAN_POINT ( 'NONE',  ( 2.500000000000000000, 1.178949249685217415, 2.041999999999998483 ) ) ;
#6701 = VERTEX_POINT ( 'NONE', #14600 ) ;
#6702 = DIRECTION ( 'NONE',  ( 0.000000000000000000, 0.000000000000000000, -1.000000000000000000 ) ) ;
#6703 = ORIENTED_EDGE ( 'NONE', *, *, #13811, .F. ) ;
#6704 = FACE_OUTER_BOUND ( 'NONE', #1765, .T. ) ;
#6705 = DIRECTION ( 'NONE',  ( -1.000000000000000000, 0.000000000000000000, 0.000000000000000000 ) ) ;
#6706 = EDGE_CURVE ( 'NONE', #588, #7659, #17788, .T. ) ;
#6707 = ORIENTED_EDGE ( 'NONE', *, *, #18678, .F. ) ;
#6708 = DIRECTION ( 'NONE',  ( 1.000000000000000000, 0.000000000000000000, 0.000000000000000000 ) ) ;
#6709 = ORIENTED_EDGE ( 'NONE', *, *, #5563, .T. ) ;
#6710 = DIRECTION ( 'NONE',  ( -1.000000000000000000, 0.000000000000000000, 0.000000000000000000 ) ) ;
#6711 = VERTEX_POINT ( 'NONE', #13016 ) ;
#6712 = EDGE_CURVE ( 'NONE', #8080, #17681, #11749, .T. ) ;
#6713 = CARTESIAN_POINT ( 'NONE',  ( 4.925000000000044231, 8.530350227276702668, -43.00000000000000000 ) ) ;
#6714 = DIRECTION ( 'NONE',  ( 0.000000000000000000, 0.000000000000000000, -1.000000000000000000 ) ) ;
#6715 = CARTESIAN_POINT ( 'NONE',  ( 9.474249098604511587, 6.330490856366296271, 15.60901600064742922 ) ) ;
#6716 = EDGE_CURVE ( 'NONE', #20034, #17803, #2184, .T. ) ;
#6717 = VERTEX_POINT ( 'NONE', #3754 ) ;
#6718 = CARTESIAN_POINT ( 'NONE',  ( 0.000000000000000000, -23.08379033237394395, 61.02926039941428371 ) ) ;
#6719 = CARTESIAN_POINT ( 'NONE',  ( 19.99999999999999645, 0.000000000000000000, 0.000000000000000000 ) ) ;
#6720 = ORIENTED_EDGE ( 'NONE', *, *, #1444, .T. ) ;
#6721 = CARTESIAN_POINT ( 'NONE',  ( -31.75000000000000000, 0.000000000000000000, 0.000000000000000000 ) ) ;
#6722 = EDGE_LOOP ( 'NONE', ( #8234, #10105, #11324, #2893 ) ) ;
#6723 = CARTESIAN_POINT ( 'NONE',  ( 12.72792205982779734, -12.72792206288791128, 15.06167500018031369 ) ) ;
#6724 = CARTESIAN_POINT ( 'NONE',  ( -6.679999999999998828, 4.605132193549069780E-15, 0.000000000000000000 ) ) ;
#6725 = DIRECTION ( 'NONE',  ( 0.000000000000000000, 1.000000000000000000, -1.287488025362403787E-15 ) ) ;
#6726 = EDGE_CURVE ( 'NONE', #2919, #1411, #5454, .T. ) ;
#6727 = EDGE_CURVE ( 'NONE', #14851, #5277, #16485, .T. ) ;
#6728 = EDGE_LOOP ( 'NONE', ( #18108, #11843, #4524, #13099 ) ) ;
#6729 = CARTESIAN_POINT ( 'NONE',  ( -3.673643420401911275, -2.497823135841289677, -0.2484800633750114396 ) ) ;
#6730 = ORIENTED_EDGE ( 'NONE', *, *, #19226, .F. ) ;
#6731 = DIRECTION ( 'NONE',  ( 0.000000000000000000, 0.000000000000000000, -1.000000000000000000 ) ) ;
#6732 = CARTESIAN_POINT ( 'NONE',  ( -24.99999999999999645, -97.49621075554985339, -111.6458212409894486 ) ) ;
#6733 = VERTEX_POINT ( 'NONE', #10555 ) ;
#6734 = PLANE ( 'NONE',  #12791 ) ;
#6735 = FACE_OUTER_BOUND ( 'NONE', #6470, .T. ) ;
#6736 = CARTESIAN_POINT ( 'NONE',  ( -10.19618095414378800, -15.25966316918061771, -11.15160624981969306 ) ) ;
#6737 = EDGE_CURVE ( 'NONE', #7841, #12500, #11826, .T. ) ;
#6738 = EDGE_LOOP ( 'NONE', ( #12513, #9495, #2577, #11492, #15522, #19616 ) ) ;
#6739 = EDGE_CURVE ( 'NONE', #10849, #18811, #5357, .T. ) ;
#6740 = DIRECTION ( 'NONE',  ( 0.000000000000000000, 0.3984010898462422290, -0.9172113015054527141 ) ) ;
#6741 = PLANE ( 'NONE',  #16179 ) ;
#6742 = AXIS2_PLACEMENT_3D ( 'NONE', #16483, #1966, #2061 ) ;
#6743 = CARTESIAN_POINT ( 'NONE',  ( -10.46442989202483709, 10.46442989454075168, -2.837166918480924949 ) ) ;
#6744 = CARTESIAN_POINT ( 'NONE',  ( 50.00000000000000000, 31.35083268962912584, 6.892027480330899929E-14 ) ) ;
#6745 = EDGE_CURVE ( 'NONE', #15579, #15761, #18398, .T. ) ;
#6746 = EDGE_CURVE ( 'NONE', #1213, #16235, #14483, .T. ) ;
#6747 = PRODUCT_RELATED_PRODUCT_CATEGORY ( 'part', '', ( #7298 ) ) ;
#6748 = ORIENTED_EDGE ( 'NONE', *, *, #5865, .F. ) ;
#6749 = LINE ( 'NONE', #800, #4151 ) ;
#6750 = DIRECTION ( 'NONE',  ( 1.000000000000000000, 0.000000000000000000, 0.000000000000000000 ) ) ;
#6751 = CARTESIAN_POINT ( 'NONE',  ( -4.248408729364577141, 6.358192988180014993, 15.98395625018030763 ) ) ;
#6752 = ORIENTED_EDGE ( 'NONE', *, *, #3124, .F. ) ;
#6753 = FACE_OUTER_BOUND ( 'NONE', #12506, .T. ) ;
#6754 = ORIENTED_EDGE ( 'NONE', *, *, #12098, .T. ) ;
#6755 = DIRECTION ( 'NONE',  ( 0.000000000000000000, 0.000000000000000000, 1.000000000000000000 ) ) ;
#6756 = CYLINDRICAL_SURFACE ( 'NONE', #15679, 8.500000000000000000 ) ;
#6757 = ORIENTED_EDGE ( 'NONE', *, *, #7368, .F. ) ;
#6758 = ADVANCED_FACE ( 'NONE', ( #13630 ), #10135, .T. ) ;
#6759 = EDGE_LOOP ( 'NONE', ( #18853, #4558 ) ) ;
#6760 = CARTESIAN_POINT ( 'NONE',  ( 47.02940313615643220, -6.215498114345216152, 80.10634491168215732 ) ) ;
#6761 = EDGE_CURVE ( 'NONE', #1320, #20501, #1689, .T. ) ;
#6762 = CYLINDRICAL_SURFACE ( 'NONE', #910, 27.60000000002759890 ) ;
#6763 = CARTESIAN_POINT ( 'NONE',  ( 0.000000000000000000, 60.35829202194874910, 24.78524934717571426 ) ) ;
#6764 = DIRECTION ( 'NONE',  ( 1.000000000000000000, 0.000000000000000000, 0.000000000000000000 ) ) ;
#6765 = EDGE_CURVE ( 'NONE', #1116, #18341, #14794, .T. ) ;
#6766 = DIRECTION ( 'NONE',  ( -1.000000000000000000, 0.000000000000000000, 0.000000000000000000 ) ) ;
#6767 = CARTESIAN_POINT ( 'NONE',  ( 6.929096493489630859, -2.870125743571144472, 16.65276250018031590 ) ) ;
#6768 = AXIS2_PLACEMENT_3D ( 'NONE', #7209, #10624, #4030 ) ;
#6769 = CARTESIAN_POINT ( 'NONE',  ( 11.17563879704981566, -2.222972771497744304, 9.664421499713199637 ) ) ;
#6770 = PRODUCT ( 'spur gear_iso_ISO - Spur gear 3M 46T 20PA 20FW ---S46C15H150L8.0S1', 'spur gear_iso_ISO - Spur gear 3M 46T 20PA 20FW ---S46C15H150L8.0S1', '', ( #10137 ) ) ;
#6771 = FACE_BOUND ( 'NONE', #8303, .T. ) ;
#6772 = DIRECTION ( 'NONE',  ( 0.000000000000000000, 0.000000000000000000, 1.000000000000000000 ) ) ;
#6773 = ORIENTED_EDGE ( 'NONE', *, *, #14493, .T. ) ;
#6774 = FACE_OUTER_BOUND ( 'NONE', #19923, .T. ) ;
#6775 = AXIS2_PLACEMENT_3D ( 'NONE', #7878, #136, #1428 ) ;
#6776 = CARTESIAN_POINT ( 'NONE',  ( 15.25966317163202746, 10.19618095047498407, 12.99995625018031475 ) ) ;
#6777 = LINE ( 'NONE', #4997, #1185 ) ;
#6778 = ORIENTED_EDGE ( 'NONE', *, *, #19207, .T. ) ;
#6779 = CARTESIAN_POINT ( 'NONE',  ( -30.00000000000000000, -85.00000000000000000, -1.040949779275250179E-14 ) ) ;
#6780 = EDGE_LOOP ( 'NONE', ( #5170, #4635, #15686, #6443, #18775 ) ) ;
#6781 = CARTESIAN_POINT ( 'NONE',  ( -4.000000000000000000, -2.309401076758531346, -5.242734410091827613 ) ) ;
#6782 = DIRECTION ( 'NONE',  ( -0.000000000000000000, 0.8660254037844392627, 0.4999999999999990008 ) ) ;
#6783 = ORIENTED_EDGE ( 'NONE', *, *, #4341, .T. ) ;
#6784 = AXIS2_PLACEMENT_3D ( 'NONE', #14852, #5092, #13057 ) ;
#6785 = ORIENTED_EDGE ( 'NONE', *, *, #2323, .T. ) ;
#6786 = CARTESIAN_POINT ( 'NONE',  ( 30.00000000000000000, -105.0000000000000000, -77.45966692414833688 ) ) ;
#6787 = DIRECTION ( 'NONE',  ( 0.000000000000000000, 0.000000000000000000, 1.000000000000000000 ) ) ;
#6788 = CARTESIAN_POINT ( 'NONE',  ( 19.99999999999999645, 0.000000000000000000, 0.000000000000000000 ) ) ;
#6789 = CARTESIAN_POINT ( 'NONE',  ( 6.929096493489624642, -2.870125743571141363, 10.38786250018031154 ) ) ;
#6790 = CARTESIAN_POINT ( 'NONE',  ( 34.82290702564237961, -118.0320511495591802, -83.30093209484321903 ) ) ;
#6791 = CIRCLE ( 'NONE', #9518, 27.60000000002760245 ) ;
#6792 = DIRECTION ( 'NONE',  ( -1.000000000000000000, -0.000000000000000000, 0.000000000000000000 ) ) ;
#6793 = DIRECTION ( 'NONE',  ( 0.000000000000000000, 0.9976687691905389288, 0.06824241336467461172 ) ) ;
#6794 = DIRECTION ( 'NONE',  ( 1.000000000000000000, 0.000000000000000000, 0.000000000000000000 ) ) ;
#6795 = ORIENTED_EDGE ( 'NONE', *, *, #17282, .F. ) ;
#6796 = EDGE_CURVE ( 'NONE', #15340, #2130, #15322, .T. ) ;
#6797 = CARTESIAN_POINT ( 'NONE',  ( 1.491842756249030399, 7.499999999820669672, 4.576981250180313765 ) ) ;
#6798 = ORIENTED_EDGE ( 'NONE', *, *, #1972, .T. ) ;
#6799 = CARTESIAN_POINT ( 'NONE',  ( -16.62983158437510056, 6.888301784570729502, 17.28051250018031482 ) ) ;
#6800 = DIRECTION ( 'NONE',  ( -1.000000000000000000, 0.000000000000000000, -0.000000000000000000 ) ) ;
#6801 = VERTEX_POINT ( 'NONE', #3974 ) ;
#6802 = DIRECTION ( 'NONE',  ( -1.000000000000000000, 0.000000000000000000, 0.000000000000000000 ) ) ;
#6803 = ORIENTED_EDGE ( 'NONE', *, *, #2332, .T. ) ;
#6804 = DIRECTION ( 'NONE',  ( 1.000000000000000000, 0.000000000000000000, 0.000000000000000000 ) ) ;
#6805 = FACE_OUTER_BOUND ( 'NONE', #19252, .T. ) ;
#6806 = ORIENTED_EDGE ( 'NONE', *, *, #11279, .T. ) ;
#6807 = PRESENTATION_LAYER_ASSIGNMENT (  '', '', ( #5158 ) ) ;
#6808 = AXIS2_PLACEMENT_3D ( 'NONE', #3344, #4832, #6616 ) ;
#6809 = AXIS2_PLACEMENT_3D ( 'NONE', #18531, #6856, #622 ) ;
#6810 = CARTESIAN_POINT ( 'NONE',  ( -6.358192987158592047, 4.248408730893246776, -12.88010624981969166 ) ) ;
#6811 = CARTESIAN_POINT ( 'NONE',  ( -10.00000000000000000, 0.000000000000000000, 0.000000000000000000 ) ) ;
#6812 = CARTESIAN_POINT ( 'NONE',  ( 8.900000000000041211, 10.82531754730546147, 166.0000000000000000 ) ) ;
#6813 = AXIS2_PLACEMENT_3D ( 'NONE', #20668, #1402, #16125 ) ;
#6814 = CARTESIAN_POINT ( 'NONE',  ( -11.17563879758428769, -2.222972768810840272, 2.060578500647426647 ) ) ;
#6815 = ORIENTED_EDGE ( 'NONE', *, *, #16599, .T. ) ;
#6816 = CARTESIAN_POINT ( 'NONE',  ( 19.99999999999999645, 64.79224928664392280, 25.14373648582975918 ) ) ;
#6817 = ORIENTED_EDGE ( 'NONE', *, *, #10110, .F. ) ;
#6818 = CIRCLE ( 'NONE', #16984, 10.00000000000000178 ) ;
#6819 = LINE ( 'NONE', #14587, #1360 ) ;
#6820 = AXIS2_PLACEMENT_3D ( 'NONE', #14023, #13910, #20358 ) ;
#6821 = ORIENTED_EDGE ( 'NONE', *, *, #20114, .F. ) ;
#6822 = EDGE_CURVE ( 'NONE', #12431, #10201, #7341, .T. ) ;
#6823 = CARTESIAN_POINT ( 'NONE',  ( -15.25966317163203279, -10.19618095047498052, 8.287456250180312622 ) ) ;
#6824 = AXIS2_PLACEMENT_3D ( 'NONE', #18975, #10494, #16950 ) ;
#6825 = CARTESIAN_POINT ( 'NONE',  ( -6.177131623262581250, 1.329966423874024758E-15, -10.85999999999999410 ) ) ;
#6826 = DIRECTION ( 'NONE',  ( -1.000000000000000000, 0.000000000000000000, -0.000000000000000000 ) ) ;
#6827 = ORIENTED_EDGE ( 'NONE', *, *, #2617, .F. ) ;
#6828 = DIRECTION ( 'NONE',  ( 1.000000000000000000, -0.000000000000000000, -0.000000000000000000 ) ) ;
#6829 = ORIENTED_EDGE ( 'NONE', *, *, #16526, .T. ) ;
#6830 = EDGE_CURVE ( 'NONE', #19485, #17488, #7001, .T. ) ;
#6831 = CYLINDRICAL_SURFACE ( 'NONE', #8212, 11.50000000000000000 ) ;
#6832 = CARTESIAN_POINT ( 'NONE',  ( 19.99999999999999645, -46.17500197033096754, 55.24372537266381045 ) ) ;
#6833 = ORIENTED_EDGE ( 'NONE', *, *, #16620, .T. ) ;
#6834 = DIRECTION ( 'NONE',  ( -1.000000000000000000, -0.000000000000000000, 0.000000000000000000 ) ) ;
#6835 = VECTOR ( 'NONE', #20543, 1000.000000000000000 ) ;
#6836 = VECTOR ( 'NONE', #14949, 1000.000000000000000 ) ;
#6837 = LINE ( 'NONE', #1982, #4840 ) ;
#6838 = AXIS2_PLACEMENT_3D ( 'NONE', #18192, #10132, #2182 ) ;
#6839 = DIRECTION ( 'NONE',  ( -0.7935941825507226710, 0.6084474286424836897, 1.243481486083094649E-31 ) ) ;
#6840 = CARTESIAN_POINT ( 'NONE',  ( -12.54593441764187745, -8.382925368423274293, 19.56919816884154528 ) ) ;
#6841 = EDGE_LOOP ( 'NONE', ( #2363, #6709, #17969, #2131 ) ) ;
#6842 = DIRECTION ( 'NONE',  ( 0.000000000000000000, 0.000000000000000000, -1.000000000000000000 ) ) ;
#6843 = VERTEX_POINT ( 'NONE', #10344 ) ;
#6844 = CARTESIAN_POINT ( 'NONE',  ( 2.943691925285397470, -14.79893867793683349, -25.51607316848092921 ) ) ;
#6845 = DIRECTION ( 'NONE',  ( 0.000000000000000000, 0.000000000000000000, 1.000000000000000000 ) ) ;
#6846 = AXIS2_PLACEMENT_3D ( 'NONE', #810, #15216, #13845 ) ;
#6847 = ORIENTED_EDGE ( 'NONE', *, *, #11447, .T. ) ;
#6848 = CIRCLE ( 'NONE', #20732, 27.60000000002759890 ) ;
#6849 = DIRECTION ( 'NONE',  ( -0.000000000000000000, -0.000000000000000000, -1.000000000000000000 ) ) ;
#6850 = LINE ( 'NONE', #7062, #16828 ) ;
#6851 = EDGE_LOOP ( 'NONE', ( #11813, #14875, #8634, #2168 ) ) ;
#6852 = ADVANCED_FACE ( 'NONE', ( #16809 ), #2293, .T. ) ;
#6854 = EDGE_CURVE ( 'NONE', #4444, #13162, #6333, .T. ) ;
#6853 = DIRECTION ( 'NONE',  ( -1.000000000000000000, -0.000000000000000000, -0.000000000000000000 ) ) ;
#6855 = VERTEX_POINT ( 'NONE', #12036 ) ;
#6856 = DIRECTION ( 'NONE',  ( -0.000000000000000000, -0.000000000000000000, -1.000000000000000000 ) ) ;
#6857 = CARTESIAN_POINT ( 'NONE',  ( -3.580422614997674557, -17.99999999956957808, 14.62973125018030984 ) ) ;
#6858 = EDGE_CURVE ( 'NONE', #20725, #18615, #2296, .T. ) ;
#6859 = VERTEX_POINT ( 'NONE', #20189 ) ;
#6860 = ORIENTED_EDGE ( 'NONE', *, *, #8907, .F. ) ;
#6861 = CARTESIAN_POINT ( 'NONE',  ( 48.03213166600498596, -4.380080863984868067, -81.79793649453739590 ) ) ;
#6862 = CARTESIAN_POINT ( 'NONE',  ( 19.99999999999999645, -10.77748419466740692, 63.93680186330469439 ) ) ;
#6863 = DIRECTION ( 'NONE',  ( 1.000000000000000000, 0.000000000000000000, 0.000000000000000000 ) ) ;
#6864 = EDGE_CURVE ( 'NONE', #15909, #6065, #258, .T. ) ;
#6865 = PRESENTATION_STYLE_ASSIGNMENT (( #413 ) ) ;
#6866 = CARTESIAN_POINT ( 'NONE',  ( 5.303300859536635770, 5.303300858261589923, -13.38942499981969014 ) ) ;
#6867 = CIRCLE ( 'NONE', #3819, 8.500000000000000000 ) ;
#6868 = AXIS2_PLACEMENT_3D ( 'NONE', #8497, #5227, #19847 ) ;
#6869 = UNCERTAINTY_MEASURE_WITH_UNIT (LENGTH_MEASURE( 1.000000000000000082E-05 ), #20342, 'distance_accuracy_value', 'NONE');
#6870 = CARTESIAN_POINT ( 'NONE',  ( -12.50000000000000533, 0.000000000000000000, 166.0000000000000000 ) ) ;
#6871 = CARTESIAN_POINT ( 'NONE',  ( -7.500000000179346316, -1.491842754445844355, 20.48166875018031519 ) ) ;
#6872 = CARTESIAN_POINT ( 'NONE',  ( -2.222972771497743416, -11.17563879704981566, 2.595671499713198660 ) ) ;
#6873 = AXIS2_PLACEMENT_3D ( 'NONE', #11477, #20915, #4805 ) ;
#6874 = CARTESIAN_POINT ( 'NONE',  ( 19.99999999999999645, 0.000000000000000000, 0.000000000000000000 ) ) ;
#6875 = DIRECTION ( 'NONE',  ( -1.000000000000000000, 0.000000000000000000, 0.000000000000000000 ) ) ;
#6876 = CIRCLE ( 'NONE', #1158, 80.00000000000000000 ) ;
#6877 = EDGE_CURVE ( 'NONE', #15833, #19592, #7696, .T. ) ;
#6878 = CIRCLE ( 'NONE', #14014, 27.60000000002759890 ) ;
#6879 = EDGE_LOOP ( 'NONE', ( #19920, #12113 ) ) ;
#6880 = DIRECTION ( 'NONE',  ( -0.000000000000000000, -0.000000000000000000, 1.000000000000000000 ) ) ;
#6881 = CARTESIAN_POINT ( 'NONE',  ( 10.19618095047497874, -15.25966317163203279, -12.91879374981968631 ) ) ;
#6882 = DIRECTION ( 'NONE',  ( -1.000000000000000000, -0.000000000000000000, -0.000000000000000000 ) ) ;
#6883 = CIRCLE ( 'NONE', #15354, 65.24900000006525147 ) ;
#6884 = ORIENTED_EDGE ( 'NONE', *, *, #9604, .F. ) ;
#6885 = CIRCLE ( 'NONE', #5890, 21.50000000000000000 ) ;
#6886 = EDGE_CURVE ( 'NONE', #9645, #4533, #12567, .T. ) ;
#6887 = DIRECTION ( 'NONE',  ( 1.000000000000000000, 0.000000000000000000, 0.000000000000000000 ) ) ;
#6888 = EDGE_LOOP ( 'NONE', ( #20590, #5612, #14863 ) ) ;
#6889 = DIRECTION ( 'NONE',  ( 1.000000000000000000, 0.000000000000000000, 0.000000000000000000 ) ) ;
#6890 = FACE_BOUND ( 'NONE', #9412, .T. ) ;
#6891 = EDGE_CURVE ( 'NONE', #6658, #12259, #16502, .T. ) ;
#6892 = ORIENTED_EDGE ( 'NONE', *, *, #1851, .T. ) ;
#6893 = ORIENTED_EDGE ( 'NONE', *, *, #10528, .T. ) ;
#6894 = FACE_OUTER_BOUND ( 'NONE', #15648, .T. ) ;
#6895 = EDGE_CURVE ( 'NONE', #17074, #9451, #8963, .T. ) ;
#6896 = VECTOR ( 'NONE', #20799, 1000.000000000000000 ) ;
#6897 = FILL_AREA_STYLE_COLOUR ( '', #3318 ) ;
#6898 = CARTESIAN_POINT ( 'NONE',  ( 4.000000000000003553, 0.3904826640788058856, -2.008738634413572465E-15 ) ) ;
#6899 = AXIS2_PLACEMENT_3D ( 'NONE', #19448, #19247, #3435 ) ;
#6900 = CARTESIAN_POINT ( 'NONE',  ( 9.999999999999998224, 59.36728637278075382, -40.73727173906726762 ) ) ;
#6901 = CARTESIAN_POINT ( 'NONE',  ( 6.929096494179676213, 2.870125741905210415, 9.209737500180313674 ) ) ;
#6902 = CARTESIAN_POINT ( 'NONE',  ( 6.177131623262577698, -10.85999999999999410, 1.329966423874025941E-15 ) ) ;
#6903 = DIRECTION ( 'NONE',  ( -1.000000000000000000, 0.000000000000000000, 0.000000000000000000 ) ) ;
#6904 = CARTESIAN_POINT ( 'NONE',  ( 4.000000000000002665, 1.935983797701078313, -5.350530693383766412 ) ) ;
#6905 = DIRECTION ( 'NONE',  ( 1.000000000000000000, 0.000000000000000000, 0.000000000000000000 ) ) ;
#6906 = ADVANCED_FACE ( 'NONE', ( #9076 ), #14266, .F. ) ;
#6907 = ORIENTED_EDGE ( 'NONE', *, *, #4006, .T. ) ;
#6908 = CARTESIAN_POINT ( 'NONE',  ( -17.50000000000000355, 0.000000000000000000, 43.00000000000000000 ) ) ;
#6909 = ORIENTED_EDGE ( 'NONE', *, *, #6895, .T. ) ;
#6910 = DIRECTION ( 'NONE',  ( -1.000000000000000000, -0.000000000000000000, 0.000000000000000000 ) ) ;
#6911 = CARTESIAN_POINT ( 'NONE',  ( -30.00000000000000000, 230.0000000000000000, 0.000000000000000000 ) ) ;
#6912 = VECTOR ( 'NONE', #16243, 1000.000000000000000 ) ;
#6913 = EDGE_LOOP ( 'NONE', ( #20867, #15781, #18576, #5961 ) ) ;
#6914 = DIRECTION ( 'NONE',  ( 1.000000000000000000, 0.000000000000000000, -0.000000000000000000 ) ) ;
#6915 = ORIENTED_EDGE ( 'NONE', *, *, #6526, .F. ) ;
#6916 = LINE ( 'NONE', #18261, #2389 ) ;
#6917 = CARTESIAN_POINT ( 'NONE',  ( 0.000000000000000000, 2.357898499370431722, -2.818925648462311528E-15 ) ) ;
#6918 = ADVANCED_FACE ( 'NONE', ( #2707 ), #2613, .T. ) ;
#6919 = ORIENTED_EDGE ( 'NONE', *, *, #10784, .T. ) ;
#6920 = CIRCLE ( 'NONE', #16728, 8.500000000000000000 ) ;
#6921 = CARTESIAN_POINT ( 'NONE',  ( 0.000000000000000000, 0.000000000000000000, -68.00000000000000000 ) ) ;
#6922 = CARTESIAN_POINT ( 'NONE',  ( -17.99999999956958163, 3.580422614997673669, -11.28901874981968945 ) ) ;
#6923 = CARTESIAN_POINT ( 'NONE',  ( -6.232800000000000118, 0.000000000000000000, 0.000000000000000000 ) ) ;
#6924 = EDGE_CURVE ( 'NONE', #5449, #18310, #9175, .T. ) ;
#6925 = DIRECTION ( 'NONE',  ( 0.000000000000000000, 0.000000000000000000, -1.000000000000000000 ) ) ;
#6926 = CARTESIAN_POINT ( 'NONE',  ( 7.902369976724399336, -7.902369978624331104, 8.245734750647425670 ) ) ;
#6927 = VERTEX_POINT ( 'NONE', #5769 ) ;
#6928 = DIRECTION ( 'NONE',  ( 1.000000000000000000, 0.000000000000000000, 0.000000000000000000 ) ) ;
#6929 = CARTESIAN_POINT ( 'NONE',  ( 6.249999999999902300, -10.82531754730554496, 126.0000000000000000 ) ) ;
#6930 = ORIENTED_EDGE ( 'NONE', *, *, #13950, .F. ) ;
#6931 = LINE ( 'NONE', #16573, #3040 ) ;
#6932 = AXIS2_PLACEMENT_3D ( 'NONE', #14888, #363, #13302 ) ;
#6933 = EDGE_LOOP ( 'NONE', ( #12931, #1835, #10041, #11228 ) ) ;
#6934 = CARTESIAN_POINT ( 'NONE',  ( 3.580422614997668340, 17.99999999956958519, 11.82183125018031333 ) ) ;
#6935 = CARTESIAN_POINT ( 'NONE',  ( 0.000000000000000000, 0.000000000000000000, 0.000000000000000000 ) ) ;
#6936 = DIRECTION ( 'NONE',  ( -0.000000000000000000, -0.000000000000000000, 1.000000000000000000 ) ) ;
#6937 = ORIENTED_EDGE ( 'NONE', *, *, #14701, .T. ) ;
#6938 = CARTESIAN_POINT ( 'NONE',  ( -6.999999999999997335, 10.52400000000000091, 0.000000000000000000 ) ) ;
#6939 = ORIENTED_EDGE ( 'NONE', *, *, #11333, .F. ) ;
#6940 = ORIENTED_EDGE ( 'NONE', *, *, #6098, .F. ) ;
#6941 = LINE ( 'NONE', #3659, #16671 ) ;
#6942 = ORIENTED_EDGE ( 'NONE', *, *, #18612, .T. ) ;
#6943 = CARTESIAN_POINT ( 'NONE',  ( 3.673643420401900173, 2.497823135841254150, -5.351519936625005691 ) ) ;
#6944 = ADVANCED_FACE ( 'NONE', ( #18716 ), #5008, .T. ) ;
#6945 = AXIS2_PLACEMENT_3D ( 'NONE', #10537, #16898, #2373 ) ;
#6946 = PRODUCT_DEFINITION_SHAPE ( 'NONE', 'NONE',  #20964 ) ;
#6947 = ADVANCED_FACE ( 'NONE', ( #2813 ), #6197, .T. ) ;
#6948 = CARTESIAN_POINT ( 'NONE',  ( 19.99999999999999645, 64.80702306891095077, 7.581672767546655756 ) ) ;
#6949 = CARTESIAN_POINT ( 'NONE',  ( -8.382925371439629458, -12.54593441562640876, 18.98013566884154812 ) ) ;
#6950 = ORIENTED_EDGE ( 'NONE', *, *, #16069, .T. ) ;
#6951 = DIRECTION ( 'NONE',  ( -1.000000000000000000, 0.000000000000000000, 0.000000000000000000 ) ) ;
#6952 = ORIENTED_EDGE ( 'NONE', *, *, #12037, .T. ) ;
#6953 = CARTESIAN_POINT ( 'NONE',  ( -5.663308646854335215, 13.67243654778934925, -21.09810441848092566 ) ) ;
#6954 = AXIS2_PLACEMENT_3D ( 'NONE', #10749, #8815, #15508 ) ;
#6955 = DIRECTION ( 'NONE',  ( -1.000000000000000000, -0.000000000000000000, -0.000000000000000000 ) ) ;
#6956 = CIRCLE ( 'NONE', #19160, 0.06721999999999977993 ) ;
#6957 = ORIENTED_EDGE ( 'NONE', *, *, #8210, .F. ) ;
#6958 = CARTESIAN_POINT ( 'NONE',  ( 0.000000000000000000, 0.000000000000000000, -130.0000000000000000 ) ) ;
#6959 = LINE ( 'NONE', #11632, #253 ) ;
#6960 = ORIENTED_EDGE ( 'NONE', *, *, #8419, .F. ) ;
#6961 = PLANE ( 'NONE',  #8891 ) ;
#6962 = ORIENTED_EDGE ( 'NONE', *, *, #12398, .T. ) ;
#6963 = DIRECTION ( 'NONE',  ( -0.000000000000000000, 0.000000000000000000, -1.000000000000000000 ) ) ;
#6964 = CARTESIAN_POINT ( 'NONE',  ( 2.163825119083639120E-09, 17.99999999999999645, 0.1977000001803091989 ) ) ;
#6965 = EDGE_LOOP ( 'NONE', ( #11081, #12832, #9268, #4993 ) ) ;
#6966 = VERTEX_POINT ( 'NONE', #4193 ) ;
#6967 = LINE ( 'NONE', #15456, #16802 ) ;
#6968 = AXIS2_PLACEMENT_3D ( 'NONE', #4245, #11985, #18659 ) ;
#6969 = FACE_OUTER_BOUND ( 'NONE', #15455, .T. ) ;
#6970 = CARTESIAN_POINT ( 'NONE',  ( 6.250000000000054179, 10.82531754730546147, -43.00000000000000000 ) ) ;
#6971 = DIRECTION ( 'NONE',  ( 0.000000000000000000, 0.000000000000000000, -1.000000000000000000 ) ) ;
#6972 = CIRCLE ( 'NONE', #16805, 27.60000000002759535 ) ;
#6973 = CIRCLE ( 'NONE', #18843, 72.00000000007199219 ) ;
#6974 = CARTESIAN_POINT ( 'NONE',  ( 6.999999999999999112, 7.118024431592597790E-15, 0.000000000000000000 ) ) ;
#6975 = CARTESIAN_POINT ( 'NONE',  ( 7.500000000000007994, -9.015933403756345817E-10, 6.638700000180315364 ) ) ;
#6976 = EDGE_CURVE ( 'NONE', #14029, #4120, #10974, .T. ) ;
#6977 = CARTESIAN_POINT ( 'NONE',  ( 10.32494394809438987, 4.276731812588564274, -10.06917225028680463 ) ) ;
#6978 = AXIS2_PLACEMENT_3D ( 'NONE', #574, #884, #17098 ) ;
#6979 = DIRECTION ( 'NONE',  ( 0.000000000000000000, 1.000000000000000000, 0.000000000000000000 ) ) ;
#6980 = DIRECTION ( 'NONE',  ( 0.000000000000000000, 0.5195839500354345608, -0.8544194045464879039 ) ) ;
#6981 = AXIS2_PLACEMENT_3D ( 'NONE', #721, #838, #8668 ) ;
#6982 = ORIENTED_EDGE ( 'NONE', *, *, #18463, .F. ) ;
#6983 = DIRECTION ( 'NONE',  ( 0.000000000000000000, -0.5195839500354227924, -0.8544194045464950094 ) ) ;
#6984 = AXIS2_PLACEMENT_3D ( 'NONE', #11234, #17709, #12937 ) ;
#6985 = CARTESIAN_POINT ( 'NONE',  ( 6.888301784570728614, 16.62983158437510056, -6.733637499819689509 ) ) ;
#6986 = DIRECTION ( 'NONE',  ( 0.000000000000000000, 0.000000000000000000, 1.000000000000000000 ) ) ;
#6987 = ADVANCED_FACE ( 'NONE', ( #18828 ), #7720, .T. ) ;
#6988 = ORIENTED_EDGE ( 'NONE', *, *, #9224, .F. ) ;
#6989 = EDGE_CURVE ( 'NONE', #12782, #5350, #11027, .T. ) ;
#6990 = DIRECTION ( 'NONE',  ( 0.000000000000000000, 0.000000000000000000, -1.000000000000000000 ) ) ;
#6991 = AXIS2_PLACEMENT_3D ( 'NONE', #12483, #7806, #7483 ) ;
#6992 = ORIENTED_EDGE ( 'NONE', *, *, #16238, .F. ) ;
#6993 = DIRECTION ( 'NONE',  ( 0.000000000000000000, 0.000000000000000000, 1.000000000000000000 ) ) ;
#6994 = CARTESIAN_POINT ( 'NONE',  ( 43.37263506394752000, -10.84340913432649600, -76.37419715032000056 ) ) ;
#6995 = PRESENTATION_LAYER_ASSIGNMENT (  '', '', ( #16807 ) ) ;
#6996 = ORIENTED_EDGE ( 'NONE', *, *, #6166, .T. ) ;
#6997 = ORIENTED_EDGE ( 'NONE', *, *, #1858, .T. ) ;
#6998 = CARTESIAN_POINT ( 'NONE',  ( -21.50000000000000000, 0.000000000000000000, -84.99999999999998579 ) ) ;
#6999 = CIRCLE ( 'NONE', #18869, 27.60000000002759890 ) ;
#7000 = FACE_OUTER_BOUND ( 'NONE', #3836, .T. ) ;
#7001 = CIRCLE ( 'NONE', #20196, 27.60000000002760245 ) ;
#7002 = CARTESIAN_POINT ( 'NONE',  ( 19.99999999999999645, 46.01927912072591198, -45.67597560296339765 ) ) ;
#7003 = EDGE_CURVE ( 'NONE', #10860, #9694, #19884, .T. ) ;
#7004 = VECTOR ( 'NONE', #4653, 1000.000000000000000 ) ;
#7005 = CARTESIAN_POINT ( 'NONE',  ( -4.248408729364575365, 6.358192988180014105, -12.29104374981968739 ) ) ;
#7006 = AXIS2_PLACEMENT_3D ( 'NONE', #12289, #1060, #14796 ) ;
#7007 = EDGE_CURVE ( 'NONE', #8524, #7867, #3428, .T. ) ;
#7008 = DIRECTION ( 'NONE',  ( -1.000000000000000000, 0.000000000000000000, 0.000000000000000000 ) ) ;
#7009 = CARTESIAN_POINT ( 'NONE',  ( 19.99999999999999645, 0.000000000000000000, 0.000000000000000000 ) ) ;
#7010 = CARTESIAN_POINT ( 'NONE',  ( 19.99999999999999645, 71.89099403602354244, 3.960426305689046522 ) ) ;
#7011 = DIRECTION ( 'NONE',  ( 0.000000000000000000, 0.7308359642781205867, 0.6825531432186576763 ) ) ;
#7012 = VERTEX_POINT ( 'NONE', #14486 ) ;
#7013 = CARTESIAN_POINT ( 'NONE',  ( -14.49999999999998934, -85.00000000000000000, 5.000000000000000000 ) ) ;
#7014 = EDGE_LOOP ( 'NONE', ( #14656, #10736, #12393, #9522 ) ) ;
#7015 = EDGE_CURVE ( 'NONE', #19691, #1598, #20213, .T. ) ;
#7016 = CARTESIAN_POINT ( 'NONE',  ( 16.62983158437509346, -6.888301784570739272, 12.56801250018031446 ) ) ;
#7017 = CARTESIAN_POINT ( 'NONE',  ( 2.985015299703225100, -21.29524168283704810, 70.66569055735612892 ) ) ;
#7018 = VECTOR ( 'NONE', #7600, 1000.000000000000000 ) ;
#7019 = EDGE_LOOP ( 'NONE', ( #8213, #17767 ) ) ;
#7020 = DIRECTION ( 'NONE',  ( 0.000000000000000000, 0.000000000000000000, 1.000000000000000000 ) ) ;
#7021 = ORIENTED_EDGE ( 'NONE', *, *, #4880, .F. ) ;
#7022 = CYLINDRICAL_SURFACE ( 'NONE', #11519, 2.649999999999999467 ) ;
#7023 = CARTESIAN_POINT ( 'NONE',  ( -15.15000000000000568, 3.245314017740485469E-16, 43.00000000000000000 ) ) ;
#7024 = VECTOR ( 'NONE', #472, 1000.000000000000000 ) ;
#7025 = ORIENTED_EDGE ( 'NONE', *, *, #88, .T. ) ;
#7026 =( GEOMETRIC_REPRESENTATION_CONTEXT ( 3 ) GLOBAL_UNCERTAINTY_ASSIGNED_CONTEXT ( ( #2010 ) ) GLOBAL_UNIT_ASSIGNED_CONTEXT ( ( #11516, #506, #8541 ) ) REPRESENTATION_CONTEXT ( 'NONE', 'WORKASPACE' ) );
#7027 = EDGE_CURVE ( 'NONE', #10438, #5556, #19544, .T. ) ;
#7028 = CARTESIAN_POINT ( 'NONE',  ( -44.00000000000000000, -85.00000000000000000, -1.040949779275250179E-14 ) ) ;
#7029 = CARTESIAN_POINT ( 'NONE',  ( -3.580422614997674557, -17.99999999956957808, -4.220268749819692466 ) ) ;
#7030 = DIRECTION ( 'NONE',  ( -0.000000000000000000, -0.000000000000000000, -1.000000000000000000 ) ) ;
#7031 = EDGE_CURVE ( 'NONE', #19744, #10678, #18533, .T. ) ;
#7032 = DIRECTION ( 'NONE',  ( -1.836909530733573776E-16, 1.000000000000000000, 0.000000000000000000 ) ) ;
#7033 = CARTESIAN_POINT ( 'NONE',  ( -4.276731815070949239, -10.32494394706616347, 0.5879222506474277576 ) ) ;
#7034 = EDGE_LOOP ( 'NONE', ( #15914, #12439 ) ) ;
#7035 = EDGE_CURVE ( 'NONE', #15733, #10469, #19219, .T. ) ;
#7036 = CARTESIAN_POINT ( 'NONE',  ( -9.850000000000019185, 0.000000000000000000, 46.00000000000000711 ) ) ;
#7037 = VERTEX_POINT ( 'NONE', #11489 ) ;
#7038 = CARTESIAN_POINT ( 'NONE',  ( 18.66082225198900701, -10.69875493221381113, -76.55584491636109590 ) ) ;
#7039 = VERTEX_POINT ( 'NONE', #12795 ) ;
#7040 = CARTESIAN_POINT ( 'NONE',  ( -2.163827323447878234E-09, -18.00000000000000000, -2.610199999819689420 ) ) ;
#7041 = DIRECTION ( 'NONE',  ( -0.000000000000000000, -0.000000000000000000, 1.000000000000000000 ) ) ;
#7042 = FACE_OUTER_BOUND ( 'NONE', #13254, .T. ) ;
#7043 = ORIENTED_EDGE ( 'NONE', *, *, #13593, .T. ) ;
#7044 = DIRECTION ( 'NONE',  ( -1.000000000000000000, 0.000000000000000000, 0.000000000000000000 ) ) ;
#7045 = ORIENTED_EDGE ( 'NONE', *, *, #5836, .T. ) ;
#7046 = DIRECTION ( 'NONE',  ( 0.000000000000000000, 0.2697967711570183891, 0.9629172873478009098 ) ) ;
#7047 = VERTEX_POINT ( 'NONE', #16169 ) ;
#7048 = VECTOR ( 'NONE', #17409, 1000.000000000000000 ) ;
#7049 = DIRECTION ( 'NONE',  ( -1.000000000000000000, 0.000000000000000000, 0.000000000000000000 ) ) ;
#7050 = DIRECTION ( 'NONE',  ( 1.000000000000000000, 0.000000000000000000, 0.000000000000000000 ) ) ;
#7051 = ITEM_DEFINED_TRANSFORMATION ( 'NONE', 'NONE', #20806,  #12461 ) ;
#7052 = CARTESIAN_POINT ( 'NONE',  ( -2.943691925285397470, 14.79893867793684059, 22.51451066884154528 ) ) ;
#7053 = ORIENTED_EDGE ( 'NONE', *, *, #14911, .T. ) ;
#7054 = CARTESIAN_POINT ( 'NONE',  ( 0.000000000000000000, -1.178949249685214307, 2.042000000000001592 ) ) ;
#7055 = ORIENTED_EDGE ( 'NONE', *, *, #1484, .T. ) ;
#7056 = CARTESIAN_POINT ( 'NONE',  ( 19.99999999999999645, 20.60847369613070512, -61.90898814327692889 ) ) ;
#7057 = CARTESIAN_POINT ( 'NONE',  ( -10.46442989454075168, -10.46442989202483709, -24.04341691848093632 ) ) ;
#7058 = DIRECTION ( 'NONE',  ( -1.000000000000000000, 0.000000000000000000, 0.000000000000000000 ) ) ;
#7059 = ORIENTED_EDGE ( 'NONE', *, *, #20198, .F. ) ;
#7060 = EDGE_CURVE ( 'NONE', #6600, #20805, #1951, .T. ) ;
#7061 = CARTESIAN_POINT ( 'NONE',  ( 33.28482093211906800, -115.9902465777789047, 81.92806195354719989 ) ) ;
#7062 = CARTESIAN_POINT ( 'NONE',  ( 2.500000000000000000, 0.000000000000000000, 2.041999999999999815 ) ) ;
#7063 = ORIENTED_EDGE ( 'NONE', *, *, #8532, .T. ) ;
#7064 = LINE ( 'NONE', #16607, #5146 ) ;
#7065 = EDGE_LOOP ( 'NONE', ( #18824, #13673, #18055, #17857, #16663 ) ) ;
#7066 = DIRECTION ( 'NONE',  ( 1.000000000000000000, 0.000000000000000000, 0.000000000000000000 ) ) ;
#7067 = CARTESIAN_POINT ( 'NONE',  ( 12.72792206288790773, 12.72792205982779912, 10.80082500018031055 ) ) ;
#7068 = ORIENTED_EDGE ( 'NONE', *, *, #26, .F. ) ;
#7069 = ORIENTED_EDGE ( 'NONE', *, *, #15174, .T. ) ;
#7070 = CARTESIAN_POINT ( 'NONE',  ( 0.2500000000000002220, 5.204748896376250699E-16, -4.250000000000000000 ) ) ;
#7071 = DIRECTION ( 'NONE',  ( 0.000000000000000000, 0.000000000000000000, 1.000000000000000000 ) ) ;
#7072 = DIRECTION ( 'NONE',  ( 0.000000000000000000, -0.000000000000000000, -1.000000000000000000 ) ) ;
#7073 = SURFACE_STYLE_USAGE ( .BOTH. , #12168 ) ;
#7074 = CARTESIAN_POINT ( 'NONE',  ( 4.248408730893249441, 6.358192987158596488, -13.68395624981969050 ) ) ;
#7075 = PRODUCT_DEFINITION_CONTEXT ( 'detailed design', #17252, 'design' ) ;
#7076 = CARTESIAN_POINT ( 'NONE',  ( 0.000000000000000000, 0.000000000000000000, 0.000000000000000000 ) ) ;
#7077 = CARTESIAN_POINT ( 'NONE',  ( 4.248408729364579806, -6.358192988180021210, 8.111356250180314476 ) ) ;
#7078 = APPLICATION_CONTEXT ( 'automotive_design' ) ;
#7079 = CARTESIAN_POINT ( 'NONE',  ( 1.343451552857795099E-09, 11.17563879731704723, -21.26135975028680036 ) ) ;
#7080 = DIRECTION ( 'NONE',  ( 0.000000000000000000, 0.000000000000000000, 1.000000000000000000 ) ) ;
#7081 = EDGE_LOOP ( 'NONE', ( #13646, #20132, #3224, #17676 ) ) ;
#7082 = EDGE_CURVE ( 'NONE', #20014, #19780, #17193, .T. ) ;
#7083 = DIRECTION ( 'NONE',  ( -1.000000000000000000, 0.000000000000000000, 0.000000000000000000 ) ) ;
#7084 = CARTESIAN_POINT ( 'NONE',  ( -2.163827323447878234E-09, -18.00000000000000000, -2.610199999819689420 ) ) ;
#7085 = CARTESIAN_POINT ( 'NONE',  ( 8.500000000000000000, 0.000000000000000000, 81.99999999999998579 ) ) ;
#7086 = EDGE_LOOP ( 'NONE', ( #13540, #16, #12934, #5681 ) ) ;
#7087 = CARTESIAN_POINT ( 'NONE',  ( 19.99999999999999645, -54.08351995568681048, -35.76369202524558233 ) ) ;
#7088 = VECTOR ( 'NONE', #8972, 1000.000000000000000 ) ;
#7089 = EDGE_LOOP ( 'NONE', ( #6056, #13745, #12262 ) ) ;
#7090 = CARTESIAN_POINT ( 'NONE',  ( 4.000000000000000000, 0.000000000000000000, -5.600000000000000533 ) ) ;
#7091 = CARTESIAN_POINT ( 'NONE',  ( 39.22505056128680678, -16.94578504268678287, -72.69725825150482024 ) ) ;
#7092 = ORIENTED_EDGE ( 'NONE', *, *, #2617, .T. ) ;
#7093 = ORIENTED_EDGE ( 'NONE', *, *, #5354, .T. ) ;
#7094 = DIRECTION ( 'NONE',  ( -1.000000000000000000, -0.000000000000000000, -0.000000000000000000 ) ) ;
#7095 = EDGE_CURVE ( 'NONE', #14158, #9402, #8107, .T. ) ;
#7096 = AXIS2_PLACEMENT_3D ( 'NONE', #8289, #18047, #14761 ) ;
#7097 = SURFACE_STYLE_FILL_AREA ( #15266 ) ;
#7098 = FACE_OUTER_BOUND ( 'NONE', #7535, .T. ) ;
#7099 = CARTESIAN_POINT ( 'NONE',  ( 19.99999999999999645, -10.77748419466740692, 63.93680186330469439 ) ) ;
#7100 = CARTESIAN_POINT ( 'NONE',  ( -7.500000000179339210, -1.491842754445842800, -14.05823124981969130 ) ) ;
#7101 = CIRCLE ( 'NONE', #16933, 72.00000000007199219 ) ;
#7102 = CARTESIAN_POINT ( 'NONE',  ( 32.00705917571151815, -113.7759157576893898, -80.64955526189534396 ) ) ;
#7103 = DIRECTION ( 'NONE',  ( 0.000000000000000000, -0.9976687691905384847, -0.06824241336468166164 ) ) ;
#7104 = CARTESIAN_POINT ( 'NONE',  ( 0.000000000000000000, 0.000000000000000000, -5.599999999999999645 ) ) ;
#7105 = DIRECTION ( 'NONE',  ( -0.5000000000000037748, -0.8660254037844364872, 0.000000000000000000 ) ) ;
#7106 = ORIENTED_EDGE ( 'NONE', *, *, #7204, .F. ) ;
#7107 = CARTESIAN_POINT ( 'NONE',  ( -6.929096493489632635, 2.870125743571140919, 2.515262500180314387 ) ) ;
#7108 = EDGE_LOOP ( 'NONE', ( #10435, #1386, #17226, #16137, #15114, #8921 ) ) ;
#7109 = CARTESIAN_POINT ( 'NONE',  ( -18.00000000000000000, 2.163826221265758884E-09, -2.158549999819688203 ) ) ;
#7110 = CARTESIAN_POINT ( 'NONE',  ( 1.457308041610579474, -21.46427008073575493, 70.59507481315790756 ) ) ;
#7111 = CIRCLE ( 'NONE', #9157, 65.24900000006525147 ) ;
#7112 = VERTEX_POINT ( 'NONE', #8005 ) ;
#7113 = CARTESIAN_POINT ( 'NONE',  ( 30.00000000000000711, 29.99999999999998579, -120.0000000000000142 ) ) ;
#7114 = EDGE_LOOP ( 'NONE', ( #3469, #14583, #16857, #5022 ) ) ;
#7115 = PRODUCT_DEFINITION_SHAPE ( 'NONE', 'NONE',  #17783 ) ;
#7116 = DIRECTION ( 'NONE',  ( -1.000000000000000000, 0.000000000000000000, 0.000000000000000000 ) ) ;
#7117 = DIRECTION ( 'NONE',  ( 0.000000000000000000, 0.000000000000000000, -1.000000000000000000 ) ) ;
#7118 = ORIENTED_EDGE ( 'NONE', *, *, #8845, .F. ) ;
#7119 = EDGE_CURVE ( 'NONE', #17864, #16324, #2639, .T. ) ;
#7120 = EDGE_CURVE ( 'NONE', #1536, #4018, #6671, .T. ) ;
#7121 = AXIS2_PLACEMENT_3D ( 'NONE', #5343, #3738, #11711 ) ;
#7122 = CARTESIAN_POINT ( 'NONE',  ( 7.500000000000004441, 1.491842754878798027, -9.345731249912210714 ) ) ;
#7123 = CARTESIAN_POINT ( 'NONE',  ( 17.99999999956957808, -3.580422614997675446, -16.00151874981969158 ) ) ;
#7124 = CYLINDRICAL_SURFACE ( 'NONE', #16387, 65.24900000006525147 ) ;
#7125 = FACE_OUTER_BOUND ( 'NONE', #1973, .T. ) ;
#7126 = EDGE_CURVE ( 'NONE', #18161, #10180, #261, .T. ) ;
#7127 = CARTESIAN_POINT ( 'NONE',  ( -11.17563879731705789, 1.343452237168309506E-09, 11.78010975064742816 ) ) ;
#7128 = EDGE_LOOP ( 'NONE', ( #18033, #6088, #2049, #9113, #3229 ) ) ;
#7129 = PLANE ( 'NONE',  #15588 ) ;
#7130 = ORIENTED_EDGE ( 'NONE', *, *, #14164, .T. ) ;
#7131 = CARTESIAN_POINT ( 'NONE',  ( 13.80207632871712775, -16.50074880709950165, -72.95245019206021198 ) ) ;
#7132 = ORIENTED_EDGE ( 'NONE', *, *, #14649, .F. ) ;
#7133 = CARTESIAN_POINT ( 'NONE',  ( -3.580422614997675002, -17.99999999956958163, 7.109331250180313866 ) ) ;
#7134 = CARTESIAN_POINT ( 'NONE',  ( 0.000000000000000000, 0.000000000000000000, 0.000000000000000000 ) ) ;
#7135 = CYLINDRICAL_SURFACE ( 'NONE', #20188, 50.00000000000001421 ) ;
#7136 = VERTEX_POINT ( 'NONE', #6713 ) ;
#7137 = EDGE_CURVE ( 'NONE', #9883, #11773, #19555, .T. ) ;
#7138 = CARTESIAN_POINT ( 'NONE',  ( 0.000000000000000000, 0.000000000000000000, 0.000000000000000000 ) ) ;
#7139 = ORIENTED_EDGE ( 'NONE', *, *, #10070, .F. ) ;
#7140 = DIRECTION ( 'NONE',  ( 0.000000000000000000, 0.000000000000000000, 1.000000000000000000 ) ) ;
#7141 = CIRCLE ( 'NONE', #19657, 65.24900000006526568 ) ;
#7142 = ORIENTED_EDGE ( 'NONE', *, *, #9798, .T. ) ;
#7143 = CARTESIAN_POINT ( 'NONE',  ( 19.99999999999999645, 46.01927912072526539, 45.67597560296404424 ) ) ;
#7144 = EDGE_CURVE ( 'NONE', #10526, #10560, #5659, .T. ) ;
#7145 = ADVANCED_FACE ( 'NONE', ( #16062 ), #14379, .T. ) ;
#7146 = ORIENTED_EDGE ( 'NONE', *, *, #10925, .F. ) ;
#7147 = AXIS2_PLACEMENT_3D ( 'NONE', #20314, #10697, #17159 ) ;
#7148 = CARTESIAN_POINT ( 'NONE',  ( 6.165580000000000283, 9.267171751443833528E-16, -7.567219999999999835 ) ) ;
#7149 = ADVANCED_FACE ( 'NONE', ( #1750 ), #11182, .T. ) ;
#7150 = CARTESIAN_POINT ( 'NONE',  ( 30.00000000000000000, -85.00000000000000000, -1.040949779275250179E-14 ) ) ;
#7151 = ITEM_DEFINED_TRANSFORMATION ( 'NONE', 'NONE', #15393,  #12461 ) ;
#7152 = CARTESIAN_POINT ( 'NONE',  ( -2.943691928843437999, -14.79893867722910450, 8.966073168841550256 ) ) ;
#7153 = VECTOR ( 'NONE', #19967, 1000.000000000000000 ) ;
#7155 = ORIENTED_EDGE ( 'NONE', *, *, #15116, .F. ) ;
#7154 = CIRCLE ( 'NONE', #1083, 72.00000000007199219 ) ;
#7156 = LINE ( 'NONE', #5263, #5883 ) ;
#7157 = AXIS2_PLACEMENT_3D ( 'NONE', #198, #5166, #1603 ) ;
#7158 = EDGE_LOOP ( 'NONE', ( #12754, #18336, #5305, #375 ) ) ;
#7159 = CARTESIAN_POINT ( 'NONE',  ( 19.99999999999999645, 0.000000000000000000, 0.000000000000000000 ) ) ;
#7160 = CARTESIAN_POINT ( 'NONE',  ( 10.46442989454075168, 10.46442989202483886, -19.33091691848093419 ) ) ;
#7161 = CARTESIAN_POINT ( 'NONE',  ( 62.49999999999999289, -30.00000000000000000, 5.000000000000000000 ) ) ;
#7162 = CIRCLE ( 'NONE', #9880, 65.24900000006526568 ) ;
#7163 = ADVANCED_FACE ( 'NONE', ( #8408 ), #14880, .T. ) ;
#7164 = ORIENTED_EDGE ( 'NONE', *, *, #15265, .F. ) ;
#7165 = DIRECTION ( 'NONE',  ( 0.000000000000000000, 0.000000000000000000, -1.000000000000000000 ) ) ;
#7166 = CARTESIAN_POINT ( 'NONE',  ( 1.084202172485504434E-14, 4.618802153517020059, -5.242734410091827613 ) ) ;
#7167 = ORIENTED_EDGE ( 'NONE', *, *, #601, .F. ) ;
#7168 = AXIS2_PLACEMENT_3D ( 'NONE', #7611, #13870, #13660 ) ;
#7169 = CARTESIAN_POINT ( 'NONE',  ( 9.319588655241851427, -21.03063704226208941, -76.26165510927667412 ) ) ;
#7170 = CIRCLE ( 'NONE', #19038, 7.500000000000000000 ) ;
#7171 = VERTEX_POINT ( 'NONE', #3532 ) ;
#7172 = CYLINDRICAL_SURFACE ( 'NONE', #2770, 72.00000000007199219 ) ;
#7173 = CARTESIAN_POINT ( 'NONE',  ( -18.00000000043040771, -3.580422610670021211, -2.453081249819692111 ) ) ;
#7174 = ORIENTED_EDGE ( 'NONE', *, *, #7095, .T. ) ;
#7175 = CIRCLE ( 'NONE', #19042, 27.60000000002759890 ) ;
#7176 = VERTEX_POINT ( 'NONE', #8506 ) ;
#7177 = DIRECTION ( 'NONE',  ( -1.000000000000000000, -0.000000000000000000, -0.000000000000000000 ) ) ;
#7178 = CARTESIAN_POINT ( 'NONE',  ( 19.99999999999999645, 0.000000000000000000, 0.000000000000000000 ) ) ;
#7179 = CYLINDRICAL_SURFACE ( 'NONE', #9889, 72.00000000007199219 ) ;
#7180 = CARTESIAN_POINT ( 'NONE',  ( -6.888301780572502864, 16.62983158603122646, 20.36323750018031120 ) ) ;
#7181 = EDGE_CURVE ( 'NONE', #10552, #8802, #1639, .T. ) ;
#7182 = DIRECTION ( 'NONE',  ( -1.000000000000000000, 0.000000000000000000, 0.000000000000000000 ) ) ;
#7183 = CARTESIAN_POINT ( 'NONE',  ( 7.500000000179346316, 1.491842754445843244, 6.344168750180314120 ) ) ;
#7184 = AXIS2_PLACEMENT_3D ( 'NONE', #11728, #16503, #2077 ) ;
#7185 = CARTESIAN_POINT ( 'NONE',  ( 6.929096493489630859, -2.870125743571144472, 16.65276250018031590 ) ) ;
#7186 = CARTESIAN_POINT ( 'NONE',  ( 4.276731812588566939, -10.32494394809438809, -7.712922250286803560 ) ) ;
#7187 = AXIS2_PLACEMENT_3D ( 'NONE', #15231, #15033, #13344 ) ;
#7188 = DIRECTION ( 'NONE',  ( -1.000000000000000000, -0.000000000000000000, 0.000000000000000000 ) ) ;
#7189 = EDGE_LOOP ( 'NONE', ( #16532, #19662, #15425, #17651 ) ) ;
#7190 = LINE ( 'NONE', #9214, #1107 ) ;
#7191 = CARTESIAN_POINT ( 'NONE',  ( 2.163825119083639534E-09, 18.00000000000000000, -7.322699999819687555 ) ) ;
#7192 = DIRECTION ( 'NONE',  ( 0.000000000000000000, 0.1361666490962400444, 0.9906859460363315328 ) ) ;
#7193 = ORIENTED_EDGE ( 'NONE', *, *, #11538, .F. ) ;
#7194 = DIRECTION ( 'NONE',  ( -0.000000000000000000, 0.000000000000000000, 1.000000000000000000 ) ) ;
#7195 = VERTEX_POINT ( 'NONE', #3839 ) ;
#7196 = DIRECTION ( 'NONE',  ( 0.000000000000000000, 0.000000000000000000, 1.000000000000000000 ) ) ;
#7197 = DIRECTION ( 'NONE',  ( -1.000000000000000000, -0.000000000000000000, -0.000000000000000000 ) ) ;
#7198 = ORIENTED_EDGE ( 'NONE', *, *, #19805, .T. ) ;
#7199 = ORIENTED_EDGE ( 'NONE', *, *, #9538, .F. ) ;
#7200 = CYLINDRICAL_SURFACE ( 'NONE', #16130, 27.60000000002760245 ) ;
#7201 = AXIS2_PLACEMENT_3D ( 'NONE', #11705, #3640, #50 ) ;
#7202 = CIRCLE ( 'NONE', #1820, 72.00000000007199219 ) ;
#7203 = CARTESIAN_POINT ( 'NONE',  ( 50.00000000000000000, 230.0000000000000000, 85.00000000000000000 ) ) ;
#7204 = EDGE_CURVE ( 'NONE', #5238, #19472, #18197, .T. ) ;
#7205 = CARTESIAN_POINT ( 'NONE',  ( 0.000000000000000000, -3.141410481201534211, 65.17333458706185922 ) ) ;
#7206 = AXIS2_PLACEMENT_3D ( 'NONE', #15972, #8030, #6423 ) ;
#7207 = CARTESIAN_POINT ( 'NONE',  ( 5.303300858261582817, -5.303300859536631329, 1.551925000180309766 ) ) ;
#7208 = CARTESIAN_POINT ( 'NONE',  ( 0.000000000000000000, -63.17103598352137794, 16.33561182745118501 ) ) ;
#7209 = CARTESIAN_POINT ( 'NONE',  ( 0.000000000000000000, 0.000000000000000000, -5.599999999999999645 ) ) ;
#7210 = EDGE_CURVE ( 'NONE', #10849, #16910, #3814, .T. ) ;
#7211 = CIRCLE ( 'NONE', #10954, 65.24900000006526568 ) ;
#7212 = LINE ( 'NONE', #655, #3073 ) ;
#7213 = CARTESIAN_POINT ( 'NONE',  ( 2.500000000000000000, -2.357898499370432166, 3.035766082959412415E-15 ) ) ;
#7214 = AXIS2_PLACEMENT_3D ( 'NONE', #9770, #120, #1718 ) ;
#7215 = ORIENTED_EDGE ( 'NONE', *, *, #16745, .T. ) ;
#7216 = CARTESIAN_POINT ( 'NONE',  ( 50.00000000000000000, -177.4842959289096029, -65.62505536500324865 ) ) ;
#7217 = ORIENTED_EDGE ( 'NONE', *, *, #3673, .F. ) ;
#7218 = CARTESIAN_POINT ( 'NONE',  ( 2.163825119083639534E-09, 18.00000000000000000, 0.1977000001803126683 ) ) ;
#7219 = CARTESIAN_POINT ( 'NONE',  ( -19.00859264729084330, -10.06624177801188758, 77.01193977728054563 ) ) ;
#7220 = ORIENTED_EDGE ( 'NONE', *, *, #16816, .T. ) ;
#7221 = CARTESIAN_POINT ( 'NONE',  ( 50.00000000000000000, -42.57363661491096707, -66.38288848018790134 ) ) ;
#7222 = EDGE_LOOP ( 'NONE', ( #16749, #15082, #16852, #20913 ) ) ;
#7223 = CYLINDRICAL_SURFACE ( 'NONE', #18996, 2.649999999999993694 ) ;
#7224 = DIRECTION ( 'NONE',  ( 0.000000000000000000, 0.000000000000000000, 1.000000000000000000 ) ) ;
#7225 = SHAPE_REPRESENTATION ( 'output shaft', ( #12461 ), #8672 ) ;
#7226 = ORIENTED_EDGE ( 'NONE', *, *, #17562, .F. ) ;
#7227 = CARTESIAN_POINT ( 'NONE',  ( 1.214306433183764966E-14, 4.618802153517020059, -5.599999999999999645 ) ) ;
#7228 = CARTESIAN_POINT ( 'NONE',  ( 19.99999999999999645, -1.971042061627920727, -64.80882494896108881 ) ) ;
#7229 = CARTESIAN_POINT ( 'NONE',  ( -6.888301780572500199, 16.62983158603121936, -9.816362499819691223 ) ) ;
#7230 = VECTOR ( 'NONE', #650, 1000.000000000000000 ) ;
#7231 = CARTESIAN_POINT ( 'NONE',  ( -4.000000000000000000, 0.000000000000000000, -5.599999999999999645 ) ) ;
#7232 = AXIS2_PLACEMENT_3D ( 'NONE', #1235, #7888, #4391 ) ;
#7233 = FACE_OUTER_BOUND ( 'NONE', #18715, .T. ) ;
#7234 = CARTESIAN_POINT ( 'NONE',  ( -2.222972768810837607, 11.17563879758428769, -14.43317149935257326 ) ) ;
#7235 = ORIENTED_EDGE ( 'NONE', *, *, #14025, .F. ) ;
#7236 = FILL_AREA_STYLE ('',( #789 ) ) ;
#7237 = DIRECTION ( 'NONE',  ( 0.000000000000000000, 0.000000000000000000, 1.000000000000000000 ) ) ;
#7238 = ORIENTED_EDGE ( 'NONE', *, *, #11333, .T. ) ;
#7239 = AXIS2_PLACEMENT_3D ( 'NONE', #9465, #17216, #4485 ) ;
#7240 = CARTESIAN_POINT ( 'NONE',  ( -0.8281006575391230973, -21.49753944123813909, -70.58133206268969673 ) ) ;
#7241 = EDGE_CURVE ( 'NONE', #13498, #7037, #9066, .T. ) ;
#7242 = ORIENTED_EDGE ( 'NONE', *, *, #9744, .T. ) ;
#7243 = ADVANCED_FACE ( 'NONE', ( #5119 ), #3637, .F. ) ;
#7244 = CARTESIAN_POINT ( 'NONE',  ( 16.62983158603122291, 6.888301780572502864, 13.29448750018031511 ) ) ;
#7245 = CARTESIAN_POINT ( 'NONE',  ( 50.00000000000000000, -170.8299878242309546, -15.48896927112552824 ) ) ;
#7246 = CARTESIAN_POINT ( 'NONE',  ( 14.50000000000000888, -85.00000000000000000, 19.00000000000000000 ) ) ;
#7247 = ORIENTED_EDGE ( 'NONE', *, *, #8561, .F. ) ;
#7248 = PLANE ( 'NONE',  #16337 ) ;
#7249 = ORIENTED_EDGE ( 'NONE', *, *, #2115, .F. ) ;
#7250 = AXIS2_PLACEMENT_3D ( 'NONE', #12854, #9963, #9859 ) ;
#7251 = LINE ( 'NONE', #10338, #7505 ) ;
#7252 = EDGE_CURVE ( 'NONE', #12463, #13263, #5533, .T. ) ;
#7253 = ORIENTED_EDGE ( 'NONE', *, *, #14142, .F. ) ;
#7254 = CYLINDRICAL_SURFACE ( 'NONE', #17022, 75.00000000000000000 ) ;
#7255 = AXIS2_PLACEMENT_3D ( 'NONE', #10898, #20641, #14199 ) ;
#7256 = DIRECTION ( 'NONE',  ( 1.000000000000000000, 0.000000000000000000, 0.000000000000000000 ) ) ;
#7257 = CARTESIAN_POINT ( 'NONE',  ( -44.00000000000000000, -85.00000000000000000, -1.040949779275250179E-14 ) ) ;
#7258 = APPLICATION_PROTOCOL_DEFINITION ( 'draft international standard', 'automotive_design', 1998, #18609 ) ;
#7259 = CARTESIAN_POINT ( 'NONE',  ( -12.54593441562641054, 8.382925371439629458, 11.91138566884154848 ) ) ;
#7260 = EDGE_CURVE ( 'NONE', #2149, #17375, #18371, .T. ) ;
#7261 = ORIENTED_EDGE ( 'NONE', *, *, #11450, .F. ) ;
#7262 = VECTOR ( 'NONE', #4928, 1000.000000000000000 ) ;
#7263 = DIRECTION ( 'NONE',  ( -1.000000000000000000, 0.000000000000000000, 0.000000000000000000 ) ) ;
#7264 = VERTEX_POINT ( 'NONE', #18478 ) ;
#7265 = DIRECTION ( 'NONE',  ( -1.000000000000000000, 0.000000000000000000, 0.000000000000000000 ) ) ;
#7266 = EDGE_CURVE ( 'NONE', #11708, #19185, #16779, .T. ) ;
#7267 = CARTESIAN_POINT ( 'NONE',  ( -10.46442989202483709, 10.46442989454075168, -21.68716691848092992 ) ) ;
#7268 = ADVANCED_FACE ( 'NONE', ( #13505 ), #780, .T. ) ;
#7269 = FACE_OUTER_BOUND ( 'NONE', #19043, .T. ) ;
#7270 = AXIS2_PLACEMENT_3D ( 'NONE', #1275, #3053, #6429 ) ;
#7271 = ORIENTED_EDGE ( 'NONE', *, *, #12468, .F. ) ;
#7272 = EDGE_CURVE ( 'NONE', #5814, #15532, #7666, .T. ) ;
#7273 = CARTESIAN_POINT ( 'NONE',  ( 31.99811442804358208, -113.7578330439423269, 80.63997760446149243 ) ) ;
#7274 = CARTESIAN_POINT ( 'NONE',  ( -1.318516776095820742, -3.857556137907092619, -5.599999999999983658 ) ) ;
#7275 = ORIENTED_EDGE ( 'NONE', *, *, #3794, .F. ) ;
#7276 = CARTESIAN_POINT ( 'NONE',  ( 14.12295668597094078, -18.21227605178592057, -77.70918423292295074 ) ) ;
#7277 = ORIENTED_EDGE ( 'NONE', *, *, #11504, .T. ) ;
#7278 = AXIS2_PLACEMENT_3D ( 'NONE', #19220, #12544, #4697 ) ;
#7279 = DIRECTION ( 'NONE',  ( 1.000000000000000000, 0.000000000000000000, 0.000000000000000000 ) ) ;
#7280 = CARTESIAN_POINT ( 'NONE',  ( -16.62983158603121936, -6.888301780572499311, -2.747612499819688914 ) ) ;
#7281 = ORIENTED_EDGE ( 'NONE', *, *, #14533, .F. ) ;
#7282 = VERTEX_POINT ( 'NONE', #20051 ) ;
#7283 = CARTESIAN_POINT ( 'NONE',  ( 46.54332301554112661, -6.983203288388267538, -86.24273042526071720 ) ) ;
#7284 = CYLINDRICAL_SURFACE ( 'NONE', #17322, 27.60000000002760245 ) ;
#7285 = DIRECTION ( 'NONE',  ( 0.000000000000000000, 0.000000000000000000, 1.000000000000000000 ) ) ;
#7286 = LINE ( 'NONE', #18859, #16315 ) ;
#7287 = EDGE_CURVE ( 'NONE', #3334, #14868, #268, .T. ) ;
#7288 = CARTESIAN_POINT ( 'NONE',  ( -16.62983158603122646, -6.888301780572501976, 18.00698750018030836 ) ) ;
#7289 = ADVANCED_FACE ( 'NONE', ( #3731, #669 ), #1324, .T. ) ;
#7290 = EDGE_CURVE ( 'NONE', #13088, #5950, #7342, .T. ) ;
#7291 = UNCERTAINTY_MEASURE_WITH_UNIT (LENGTH_MEASURE( 1.000000000000000082E-05 ), #16732, 'distance_accuracy_value', 'NONE');
#7292 = VECTOR ( 'NONE', #19307, 1000.000000000000000 ) ;
#7293 = FILL_AREA_STYLE_COLOUR ( '', #2464 ) ;
#7294 = CARTESIAN_POINT ( 'NONE',  ( -4.248408730893249441, -6.358192987158595599, 0.4535437501803143978 ) ) ;
#7295 = CARTESIAN_POINT ( 'NONE',  ( 30.00000000000000000, -85.00000000000000000, -1.040949779275250179E-14 ) ) ;
#7296 = CIRCLE ( 'NONE', #14754, 27.60000000002759535 ) ;
#7297 = CARTESIAN_POINT ( 'NONE',  ( 2.222972771497739419, 11.17563879704981922, -11.54182850028680640 ) ) ;
#7298 = PRODUCT ( 'tail shaft', 'tail shaft', '', ( #500 ) ) ;
#7299 = EDGE_CURVE ( 'NONE', #20061, #20910, #4272, .T. ) ;
#7300 = DIRECTION ( 'NONE',  ( 0.000000000000000000, 0.000000000000000000, 1.000000000000000000 ) ) ;
#7301 = ORIENTED_EDGE ( 'NONE', *, *, #17537, .F. ) ;
#7302 = FACE_OUTER_BOUND ( 'NONE', #11821, .T. ) ;
#7303 = CARTESIAN_POINT ( 'NONE',  ( -3.580422614997675002, -17.99999999956958163, -11.74066874981969200 ) ) ;
#7304 = FACE_OUTER_BOUND ( 'NONE', #14599, .T. ) ;
#7305 = EDGE_LOOP ( 'NONE', ( #3253, #16436, #15370, #20735 ) ) ;
#7306 = DIRECTION ( 'NONE',  ( -1.000000000000000000, -0.000000000000000000, -0.000000000000000000 ) ) ;
#7307 = ORIENTED_EDGE ( 'NONE', *, *, #6478, .F. ) ;
#7308 = DIRECTION ( 'NONE',  ( 1.000000000000000000, 0.000000000000000000, -0.000000000000000000 ) ) ;
#7309 = FACE_OUTER_BOUND ( 'NONE', #10689, .T. ) ;
#7310 = ORIENTED_EDGE ( 'NONE', *, *, #13385, .T. ) ;
#7311 = ORIENTED_EDGE ( 'NONE', *, *, #11837, .T. ) ;
#7312 = DIRECTION ( 'NONE',  ( 1.000000000000000000, 0.000000000000000000, 0.000000000000000000 ) ) ;
#7313 = CIRCLE ( 'NONE', #1903, 27.60000000002760245 ) ;
#7314 = DIRECTION ( 'NONE',  ( 0.000000000000000000, 0.000000000000000000, 1.000000000000000000 ) ) ;
#7315 = CIRCLE ( 'NONE', #4288, 65.24900000006525147 ) ;
#7316 = CARTESIAN_POINT ( 'NONE',  ( 0.000000000000000000, 0.000000000000000000, 68.00000000000000000 ) ) ;
#7317 = CIRCLE ( 'NONE', #18549, 72.00000000007199219 ) ;
#7318 = CARTESIAN_POINT ( 'NONE',  ( 1.491842756249028845, 7.499999999820661678, -11.11291874981969308 ) ) ;
#7319 = CIRCLE ( 'NONE', #6984, 0.06721999999999977993 ) ;
#7320 = DIRECTION ( 'NONE',  ( 1.000000000000000000, 0.000000000000000000, -0.000000000000000000 ) ) ;
#7321 = CYLINDRICAL_SURFACE ( 'NONE', #2722, 27.60000000002759535 ) ;
#7322 = CARTESIAN_POINT ( 'NONE',  ( 2.500000000000000000, 2.357898499370433054, -1.951563910473907981E-15 ) ) ;
#7323 = DIRECTION ( 'NONE',  ( 0.000000000000000000, 0.000000000000000000, 1.000000000000000000 ) ) ;
#7324 = AXIS2_PLACEMENT_3D ( 'NONE', #14769, #1741, #8195 ) ;
#7325 = AXIS2_PLACEMENT_3D ( 'NONE', #11915, #9069, #2492 ) ;
#7326 = ORIENTED_EDGE ( 'NONE', *, *, #3483, .T. ) ;
#7327 = CARTESIAN_POINT ( 'NONE',  ( 2.500000000000000000, 2.357898499370431722, -2.818925648462311528E-15 ) ) ;
#7328 = ORIENTED_EDGE ( 'NONE', *, *, #1872, .F. ) ;
#7329 = CARTESIAN_POINT ( 'NONE',  ( -12.72792206288791128, -12.72792205982779912, 6.088325000180314639 ) ) ;
#7330 = CARTESIAN_POINT ( 'NONE',  ( 3.744012722225321443, -21.17498532244396614, 70.71631193418075156 ) ) ;
#7331 = ORIENTED_EDGE ( 'NONE', *, *, #1173, .F. ) ;
#7332 = EDGE_CURVE ( 'NONE', #3623, #12159, #5965, .T. ) ;
#7333 = DIRECTION ( 'NONE',  ( -1.000000000000000000, 0.000000000000000000, -0.000000000000000000 ) ) ;
#7334 = VERTEX_POINT ( 'NONE', #10529 ) ;
#7335 = DIRECTION ( 'NONE',  ( 0.000000000000000000, 0.000000000000000000, -1.000000000000000000 ) ) ;
#7336 = DIRECTION ( 'NONE',  ( 0.000000000000000000, 0.000000000000000000, 1.000000000000000000 ) ) ;
#7337 = DIRECTION ( 'NONE',  ( 1.000000000000000000, 0.000000000000000000, 0.000000000000000000 ) ) ;
#7338 = EDGE_CURVE ( 'NONE', #10026, #5060, #10751, .T. ) ;
#7339 = ORIENTED_EDGE ( 'NONE', *, *, #4406, .T. ) ;
#7340 = CARTESIAN_POINT ( 'NONE',  ( -24.99999999999999289, -84.99999999999998579, -75.00000000000001421 ) ) ;
#7341 = CIRCLE ( 'NONE', #17512, 27.60000000002759890 ) ;
#7342 = LINE ( 'NONE', #2896, #1303 ) ;
#7343 = CARTESIAN_POINT ( 'NONE',  ( 16.62983158437509346, -6.888301784570737496, -15.70698749981969122 ) ) ;
#7344 = CARTESIAN_POINT ( 'NONE',  ( 30.43430782549248903, -42.57363661491096707, -66.38288848018790134 ) ) ;
#7345 = VECTOR ( 'NONE', #3348, 1000.000000000000000 ) ;
#7346 = CIRCLE ( 'NONE', #17853, 10.85999999999999410 ) ;
#7347 = CARTESIAN_POINT ( 'NONE',  ( 3.599999999999902833, -10.82531754730554496, 40.00000000000000000 ) ) ;
#7348 = CARTESIAN_POINT ( 'NONE',  ( -11.17563879731705789, 1.343452237168309506E-09, -7.069890249352571487 ) ) ;
#7349 = ORIENTED_EDGE ( 'NONE', *, *, #6858, .T. ) ;
#7350 = PRESENTATION_STYLE_ASSIGNMENT (( #18595 ) ) ;
#7351 = CARTESIAN_POINT ( 'NONE',  ( -24.99999999999999289, -40.41646384503850697, -66.42520834682601105 ) ) ;
#7352 = EDGE_LOOP ( 'NONE', ( #21, #15886, #356 ) ) ;
#7353 = CARTESIAN_POINT ( 'NONE',  ( 15.37884418493265848, -15.02891098528240654, -73.77646566961475116 ) ) ;
#7354 = ORIENTED_EDGE ( 'NONE', *, *, #12600, .F. ) ;
#7355 = VECTOR ( 'NONE', #9393, 1000.000000000000000 ) ;
#7356 = CARTESIAN_POINT ( 'NONE',  ( 15.25966317163202746, 10.19618095047498407, -5.850043749819688443 ) ) ;
#7357 = DIRECTION ( 'NONE',  ( 0.000000000000000000, -0.4999999999999992784, 0.8660254037844389297 ) ) ;
#7358 = CARTESIAN_POINT ( 'NONE',  ( 0.000000000000000000, 0.000000000000000000, 46.00000000000000711 ) ) ;
#7359 = ORIENTED_EDGE ( 'NONE', *, *, #2330, .F. ) ;
#7360 = AXIS2_PLACEMENT_3D ( 'NONE', #3549, #1101, #11820 ) ;
#7361 = CARTESIAN_POINT ( 'NONE',  ( 50.00000000000000000, -127.3290820621008947, 85.00000000000000000 ) ) ;
#7362 = VERTEX_POINT ( 'NONE', #20486 ) ;
#7363 = DIRECTION ( 'NONE',  ( -1.000000000000000000, -0.000000000000000000, 0.000000000000000000 ) ) ;
#7364 = EDGE_CURVE ( 'NONE', #3116, #15567, #17158, .T. ) ;
#7365 = ORIENTED_EDGE ( 'NONE', *, *, #9843, .T. ) ;
#7366 =( REPRESENTATION_RELATIONSHIP ('NONE','NONE', #13739, #2344 ) REPRESENTATION_RELATIONSHIP_WITH_TRANSFORMATION ( #14175 )SHAPE_REPRESENTATION_RELATIONSHIP( ) );
#7367 = CARTESIAN_POINT ( 'NONE',  ( 19.99999999999999645, 1.971042061628357933, 64.80882494896107460 ) ) ;
#7368 = EDGE_CURVE ( 'NONE', #7828, #9385, #1963, .T. ) ;
#7369 = DIRECTION ( 'NONE',  ( 0.000000000000000000, 0.000000000000000000, 1.000000000000000000 ) ) ;
#7370 = CARTESIAN_POINT ( 'NONE',  ( -8.382925371439629458, -12.54593441562640876, 0.1301356688415446494 ) ) ;
#7371 = ORIENTED_EDGE ( 'NONE', *, *, #16216, .F. ) ;
#7372 = CARTESIAN_POINT ( 'NONE',  ( -4.000000000000000000, -1.933795701539610334, -5.351162342337702604 ) ) ;
#7373 = ORIENTED_EDGE ( 'NONE', *, *, #10229, .T. ) ;
#7374 = ADVANCED_FACE ( 'NONE', ( #15825 ), #7768, .F. ) ;
#7375 = CARTESIAN_POINT ( 'NONE',  ( 9.999999999999998224, 0.9548212943365428362, 71.99366858485716136 ) ) ;
#7376 = CARTESIAN_POINT ( 'NONE',  ( 6.888301780572505528, -16.62983158603121581, 13.74613750018031233 ) ) ;
#7377 = CARTESIAN_POINT ( 'NONE',  ( 19.99999999999999645, 0.000000000000000000, 0.000000000000000000 ) ) ;
#7378 = CARTESIAN_POINT ( 'NONE',  ( 19.99999999999999645, 0.000000000000000000, 0.000000000000000000 ) ) ;
#7379 = EDGE_LOOP ( 'NONE', ( #7167, #1017, #16050, #3409 ) ) ;
#7380 = CARTESIAN_POINT ( 'NONE',  ( 0.000000000000000000, 0.000000000000000000, -90.00000000000000000 ) ) ;
#7381 = CARTESIAN_POINT ( 'NONE',  ( 30.00000000000000000, -110.0000000000000142, 44.99999999999999289 ) ) ;
#7382 = ORIENTED_EDGE ( 'NONE', *, *, #19816, .F. ) ;
#7383 = CARTESIAN_POINT ( 'NONE',  ( 30.00000000000000000, -39.99999999999999289, 49.89999999999999858 ) ) ;
#7384 = ORIENTED_EDGE ( 'NONE', *, *, #4497, .T. ) ;
#7385 = CARTESIAN_POINT ( 'NONE',  ( 19.99999999999999645, -49.77519642624036322, 42.18840861821767163 ) ) ;
#7386 = CARTESIAN_POINT ( 'NONE',  ( -16.62983158437509701, 6.888301784570728614, -20.41948749981969158 ) ) ;
#7387 = ORIENTED_EDGE ( 'NONE', *, *, #4642, .F. ) ;
#7388 = ORIENTED_EDGE ( 'NONE', *, *, #20685, .T. ) ;
#7389 = CARTESIAN_POINT ( 'NONE',  ( 7.000000000000000888, -11.17999999999998550, 1.388749470233097582E-15 ) ) ;
#7390 = ADVANCED_FACE ( 'NONE', ( #15404 ), #1109, .T. ) ;
#7391 = CARTESIAN_POINT ( 'NONE',  ( 5.000000000000000888, 4.250000000000000000, 0.000000000000000000 ) ) ;
#7392 = EDGE_CURVE ( 'NONE', #1631, #13026, #20180, .T. ) ;
#7393 = CARTESIAN_POINT ( 'NONE',  ( 0.000000000000000000, -10.74906464462166866, 71.19310085447965264 ) ) ;
#7394 = LINE ( 'NONE', #15663, #19372 ) ;
#7395 =( NAMED_UNIT ( * ) SI_UNIT ( $, .STERADIAN. ) SOLID_ANGLE_UNIT ( ) );
#7396 = CARTESIAN_POINT ( 'NONE',  ( 18.00000000000000355, -2.163824016901520597E-09, 13.88355000018031049 ) ) ;
#7397 = EDGE_CURVE ( 'NONE', #1369, #10946, #20231, .T. ) ;
#7398 = CARTESIAN_POINT ( 'NONE',  ( -7.499999999820669672, 1.491842756249032620, 2.220731250180314476 ) ) ;
#7399 = ADVANCED_FACE ( 'NONE', ( #12543 ), #7443, .T. ) ;
#7400 = ORIENTED_EDGE ( 'NONE', *, *, #7693, .T. ) ;
#7401 = PRODUCT_RELATED_PRODUCT_CATEGORY ( 'part', '', ( #12039 ) ) ;
#7402 = CARTESIAN_POINT ( 'NONE',  ( -5.303300859536636658, -5.303300858261589035, 19.59807500018031590 ) ) ;
#7403 = CARTESIAN_POINT ( 'NONE',  ( 8.382925371439627682, 12.54593441562639988, 18.07455183151907363 ) ) ;
#7404 = CARTESIAN_POINT ( 'NONE',  ( -52.49999999999999289, -120.0000000000000142, 0.000000000000000000 ) ) ;
#7405 = EDGE_LOOP ( 'NONE', ( #14396, #5399, #331, #2666 ) ) ;
#7406 = CARTESIAN_POINT ( 'NONE',  ( 7.500000000000000000, 9.184850993605147944E-16, 40.00000000000000000 ) ) ;
#7407 = CARTESIAN_POINT ( 'NONE',  ( 10.19618095414378800, 15.25966316918061416, -15.86410624981969342 ) ) ;
#7408 = CARTESIAN_POINT ( 'NONE',  ( 30.00000000000000000, -47.51018795805313033, -71.56352010304497924 ) ) ;
#7409 = EDGE_CURVE ( 'NONE', #8346, #2456, #2584, .T. ) ;
#7410 = ORIENTED_EDGE ( 'NONE', *, *, #3170, .T. ) ;
#7411 = EDGE_CURVE ( 'NONE', #15579, #4783, #17313, .T. ) ;
#7412 = CARTESIAN_POINT ( 'NONE',  ( -10.00000000000000000, 0.000000000000000000, 0.000000000000000000 ) ) ;
#7413 = ORIENTED_EDGE ( 'NONE', *, *, #9840, .F. ) ;
#7414 = CARTESIAN_POINT ( 'NONE',  ( 6.250000000000054179, 10.82531754730546147, 43.00000000000000000 ) ) ;
#7415 = DIRECTION ( 'NONE',  ( 0.000000000000000000, 0.000000000000000000, 1.000000000000000000 ) ) ;
#7416 = ORIENTED_EDGE ( 'NONE', *, *, #12825, .F. ) ;
#7417 = ORIENTED_EDGE ( 'NONE', *, *, #3635, .F. ) ;
#7418 = DIRECTION ( 'NONE',  ( -0.000000000000000000, -0.000000000000000000, 1.000000000000000000 ) ) ;
#7419 = EDGE_CURVE ( 'NONE', #6250, #19812, #20376, .T. ) ;
#7420 = CYLINDRICAL_SURFACE ( 'NONE', #19400, 2.649999999999994582 ) ;
#7421 = EDGE_CURVE ( 'NONE', #4938, #20704, #13137, .T. ) ;
#7422 = CYLINDRICAL_SURFACE ( 'NONE', #4097, 17.50000000000000355 ) ;
#7423 = CARTESIAN_POINT ( 'NONE',  ( -6.358192988180014993, -4.248408729364575365, -5.222293749819688635 ) ) ;
#7424 = CARTESIAN_POINT ( 'NONE',  ( 19.99999999999999645, 45.48683723007275148, -46.78012013466171481 ) ) ;
#7425 = CARTESIAN_POINT ( 'NONE',  ( 43.62500077266424370, -124.9999999999999858, -90.00000000000001421 ) ) ;
#7426 = DIRECTION ( 'NONE',  ( -0.1159034202170342726, 1.393303357259140646E-11, -0.9932604880805404601 ) ) ;
#7427 = DIRECTION ( 'NONE',  ( 1.000000000000000000, 0.000000000000000000, 0.000000000000000000 ) ) ;
#7428 = AXIS2_PLACEMENT_3D ( 'NONE', #15536, #15221, #9085 ) ;
#7429 = ORIENTED_EDGE ( 'NONE', *, *, #14933, .T. ) ;
#7430 = DIRECTION ( 'NONE',  ( 0.000000000000000000, 0.000000000000000000, -1.000000000000000000 ) ) ;
#7431 = ORIENTED_EDGE ( 'NONE', *, *, #2294, .F. ) ;
#7432 = CARTESIAN_POINT ( 'NONE',  ( -12.72792205982779912, 12.72792206288790950, 8.444575000180313040 ) ) ;
#7433 = CARTESIAN_POINT ( 'NONE',  ( 0.000000000000000000, 0.000000000000000000, 81.99999999999998579 ) ) ;
#7434 = VERTEX_POINT ( 'NONE', #9051 ) ;
#7435 = EDGE_CURVE ( 'NONE', #2489, #18656, #8998, .T. ) ;
#7436 = CARTESIAN_POINT ( 'NONE',  ( 19.99999999999999645, 59.31169354540738681, 27.19476070466876649 ) ) ;
#7437 = ORIENTED_EDGE ( 'NONE', *, *, #16966, .T. ) ;
#7438 = CARTESIAN_POINT ( 'NONE',  ( -7.500000000000000000, 0.000000000000000000, 166.0000000000000000 ) ) ;
#7439 = CYLINDRICAL_SURFACE ( 'NONE', #16150, 27.60000000002759535 ) ;
#7440 = CARTESIAN_POINT ( 'NONE',  ( 19.99999999999999645, -35.35772184876915958, 54.34979580218180928 ) ) ;
#7441 = ORIENTED_EDGE ( 'NONE', *, *, #1986, .T. ) ;
#7442 = CARTESIAN_POINT ( 'NONE',  ( 4.248408729364579806, -6.358192988180021210, -20.16364374981968766 ) ) ;
#7443 = CYLINDRICAL_SURFACE ( 'NONE', #11110, 27.60000000002759890 ) ;
#7444 = DIRECTION ( 'NONE',  ( -1.000000000000000000, -0.000000000000000000, -0.000000000000000000 ) ) ;
#7445 = DIRECTION ( 'NONE',  ( -0.000000000000000000, -0.000000000000000000, 1.000000000000000000 ) ) ;
#7446 = ADVANCED_BREP_SHAPE_REPRESENTATION ( '', ( #10096, #12461 ), #7026 ) ;
#7447 = VECTOR ( 'NONE', #16997, 1000.000000000000000 ) ;
#7448 = DIRECTION ( 'NONE',  ( 1.000000000000000000, 0.000000000000000000, 0.000000000000000000 ) ) ;
#7449 = ORIENTED_EDGE ( 'NONE', *, *, #778, .F. ) ;
#7450 = ADVANCED_FACE ( 'NONE', ( #1802 ), #16217, .F. ) ;
#7451 = DIRECTION ( 'NONE',  ( -0.000000000000000000, -1.000000000000000000, -0.000000000000000000 ) ) ;
#7452 = ORIENTED_EDGE ( 'NONE', *, *, #7287, .T. ) ;
#7453 = CARTESIAN_POINT ( 'NONE',  ( 7.417002224176414416, -20.23665979631132572, -71.11836349014900804 ) ) ;
#7454 = DIRECTION ( 'NONE',  ( -1.000000000000000000, 0.000000000000000000, 0.000000000000000000 ) ) ;
#7455 = VERTEX_POINT ( 'NONE', #2007 ) ;
#7456 = CARTESIAN_POINT ( 'NONE',  ( -12.72792205982779912, 12.72792206288790950, -17.92582499981968880 ) ) ;
#7457 = DIRECTION ( 'NONE',  ( -1.000000000000000000, 0.000000000000000000, 0.000000000000000000 ) ) ;
#7458 = DIRECTION ( 'NONE',  ( 0.8191520442889896891, 0.000000000000000000, 0.5735764363510490460 ) ) ;
#7459 = ORIENTED_EDGE ( 'NONE', *, *, #1796, .F. ) ;
#7460 = CARTESIAN_POINT ( 'NONE',  ( -6.999999999999995559, 4.546351088565595293E-15, 0.000000000000000000 ) ) ;
#7461 = VERTEX_POINT ( 'NONE', #8151 ) ;
#7462 = DIRECTION ( 'NONE',  ( 0.8660254037844354880, -0.5000000000000055511, 0.000000000000000000 ) ) ;
#7463 = CIRCLE ( 'NONE', #357, 2.649999999999999467 ) ;
#7464 = ORIENTED_EDGE ( 'NONE', *, *, #16599, .F. ) ;
#7465 = VECTOR ( 'NONE', #3926, 1000.000000000000000 ) ;
#7466 = AXIS2_PLACEMENT_3D ( 'NONE', #6062, #6379, #15713 ) ;
#7467 = CARTESIAN_POINT ( 'NONE',  ( 19.99999999999999645, -63.17103598352115057, -16.33561182745204476 ) ) ;
#7468 = PRODUCT ( 'Sealed Cast Iron Gearbox Casing', 'Sealed Cast Iron Gearbox Casing', '', ( #12041 ) ) ;
#7469 = DIRECTION ( 'NONE',  ( 0.000000000000000000, 0.000000000000000000, -1.000000000000000000 ) ) ;
#7470 = ITEM_DEFINED_TRANSFORMATION ( 'NONE', 'NONE', #1206,  #12461 ) ;
#7471 = CARTESIAN_POINT ( 'NONE',  ( -5.663308650141539502, -13.67243654642775574, -0.1643955811584559001 ) ) ;
#7472 = VERTEX_POINT ( 'NONE', #14240 ) ;
#7473 = ADVANCED_FACE ( 'NONE', ( #18010 ), #20686, .T. ) ;
#7474 = DIRECTION ( 'NONE',  ( -1.000000000000000000, -0.000000000000000000, 0.000000000000000000 ) ) ;
#7475 = EDGE_LOOP ( 'NONE', ( #18876, #1476, #5638, #13612 ) ) ;
#7476 = CARTESIAN_POINT ( 'NONE',  ( 9.999999999999998224, -63.48283426024829623, -33.96954156735433372 ) ) ;
#7477 = AXIS2_PLACEMENT_3D ( 'NONE', #13539, #18413, #19893 ) ;
#7478 = CARTESIAN_POINT ( 'NONE',  ( 3.580422614997667896, 17.99999999956958163, 9.917231250180309488 ) ) ;
#7479 = DIRECTION ( 'NONE',  ( -1.000000000000000000, -0.000000000000000000, -0.000000000000000000 ) ) ;
#7480 = AXIS2_PLACEMENT_3D ( 'NONE', #19411, #11558, #6471 ) ;
#7481 = LINE ( 'NONE', #10168, #17143 ) ;
#7482 = ORIENTED_EDGE ( 'NONE', *, *, #3851, .F. ) ;
#7483 = DIRECTION ( 'NONE',  ( 0.000000000000000000, 0.000000000000000000, 1.000000000000000000 ) ) ;
#7484 = DIRECTION ( 'NONE',  ( -0.000000000000000000, -0.000000000000000000, -1.000000000000000000 ) ) ;
#7485 = VERTEX_POINT ( 'NONE', #1704 ) ;
#7486 = CARTESIAN_POINT ( 'NONE',  ( 20.50516414656735265, -10.42283242499551932, -83.08857956002572109 ) ) ;
#7487 = DIRECTION ( 'NONE',  ( -1.000000000000000000, 0.000000000000000000, 0.000000000000000000 ) ) ;
#7488 = CARTESIAN_POINT ( 'NONE',  ( -10.19618095414378445, -15.25966316918061239, -3.631206249819690868 ) ) ;
#7489 = EDGE_LOOP ( 'NONE', ( #9666, #20715 ) ) ;
#7490 = ORIENTED_EDGE ( 'NONE', *, *, #15962, .T. ) ;
#7491 = DIRECTION ( 'NONE',  ( -0.000000000000000000, -0.000000000000000000, -1.000000000000000000 ) ) ;
#7492 =( GEOMETRIC_REPRESENTATION_CONTEXT ( 3 ) GLOBAL_UNCERTAINTY_ASSIGNED_CONTEXT ( ( #955 ) ) GLOBAL_UNIT_ASSIGNED_CONTEXT ( ( #18012, #7962, #16122 ) ) REPRESENTATION_CONTEXT ( 'NONE', 'WORKASPACE' ) );
#7493 = CIRCLE ( 'NONE', #14618, 27.60000000002759890 ) ;
#7494 = PLANE ( 'NONE',  #8847 ) ;
#7495 = DIRECTION ( 'NONE',  ( 1.000000000000000000, 0.000000000000000000, 0.000000000000000000 ) ) ;
#7496 = FACE_OUTER_BOUND ( 'NONE', #19942, .T. ) ;
#7497 = AXIS2_PLACEMENT_3D ( 'NONE', #1153, #1041, #20633 ) ;
#7498 =( NAMED_UNIT ( * ) PLANE_ANGLE_UNIT ( ) SI_UNIT ( $, .RADIAN. ) );
#7499 = CARTESIAN_POINT ( 'NONE',  ( 16.62983158603122646, 6.888301780572504640, 13.29448750018031156 ) ) ;
#7500 = CARTESIAN_POINT ( 'NONE',  ( -2.500000000000002220, 3.061616997868386099E-16, -5.600000000000000533 ) ) ;
#7501 = EDGE_LOOP ( 'NONE', ( #5168, #13481, #12119, #15282, #3134 ) ) ;
#7502 = LINE ( 'NONE', #5487, #10407 ) ;
#7503 = CARTESIAN_POINT ( 'NONE',  ( -8.382925371439625906, -12.54593441562639988, 13.36205183151907505 ) ) ;
#7504 = CARTESIAN_POINT ( 'NONE',  ( -39.99999999999999289, -40.00000000000000000, -130.0000000000000000 ) ) ;
#7505 = VECTOR ( 'NONE', #20285, 1000.000000000000000 ) ;
#7506 = EDGE_CURVE ( 'NONE', #17111, #10885, #13766, .T. ) ;
#7507 = ORIENTED_EDGE ( 'NONE', *, *, #12601, .T. ) ;
#7508 = CARTESIAN_POINT ( 'NONE',  ( 19.99999999999999645, -71.89099403602351401, -3.960426305689549675 ) ) ;
#7509 = ADVANCED_FACE ( 'NONE', ( #102 ), #18500, .T. ) ;
#7510 = CARTESIAN_POINT ( 'NONE',  ( 6.888301780572507305, -16.62983158603121936, -22.04926249981969022 ) ) ;
#7511 = CARTESIAN_POINT ( 'NONE',  ( 20.55500000000001748, 0.000000000000000000, 0.000000000000000000 ) ) ;
#7512 = AXIS2_PLACEMENT_3D ( 'NONE', #10816, #9118, #15787 ) ;
#7513 = ORIENTED_EDGE ( 'NONE', *, *, #15191, .T. ) ;
#7514 = FACE_OUTER_BOUND ( 'NONE', #13371, .T. ) ;
#7515 = ORIENTED_EDGE ( 'NONE', *, *, #6739, .F. ) ;
#7516 = CARTESIAN_POINT ( 'NONE',  ( 19.99999999999999645, 45.48683723007212620, 46.78012013466234720 ) ) ;
#7517 = LINE ( 'NONE', #14003, #6533 ) ;
#7518 = VERTEX_POINT ( 'NONE', #19597 ) ;
#7519 = EDGE_CURVE ( 'NONE', #16575, #20492, #9027, .T. ) ;
#7520 = ORIENTED_EDGE ( 'NONE', *, *, #14376, .F. ) ;
#7521 = FACE_OUTER_BOUND ( 'NONE', #6604, .T. ) ;
#7522 = DIRECTION ( 'NONE',  ( -1.000000000000000000, 0.000000000000000000, 0.000000000000000000 ) ) ;
#7523 = VECTOR ( 'NONE', #19998, 1000.000000000000000 ) ;
#7524 = VECTOR ( 'NONE', #10489, 1000.000000000000000 ) ;
#7525 = AXIS2_PLACEMENT_3D ( 'NONE', #19371, #14717, #17800 ) ;
#7526 = LINE ( 'NONE', #14220, #6185 ) ;
#7527 = AXIS2_PLACEMENT_3D ( 'NONE', #16279, #19771, #172 ) ;
#7528 = EDGE_CURVE ( 'NONE', #19132, #14670, #2933, .T. ) ;
#7529 = CARTESIAN_POINT ( 'NONE',  ( -11.17563879758427525, -2.222972768810838051, 13.78785899971320106 ) ) ;
#7530 = CYLINDRICAL_SURFACE ( 'NONE', #15967, 63.70999227554992217 ) ;
#7531 = AXIS2_PLACEMENT_3D ( 'NONE', #4079, #5566, #7263 ) ;
#7532 = DIRECTION ( 'NONE',  ( -1.000000000000000000, -0.000000000000000000, 0.000000000000000000 ) ) ;
#7533 = DIRECTION ( 'NONE',  ( 0.000000000000000000, -0.000000000000000000, 1.000000000000000000 ) ) ;
#7534 = EDGE_CURVE ( 'NONE', #232, #5038, #20866, .T. ) ;
#7535 = EDGE_LOOP ( 'NONE', ( #15768, #15963, #20845, #515 ) ) ;
#7536 = CYLINDRICAL_SURFACE ( 'NONE', #19347, 80.00000000000000000 ) ;
#7537 = EDGE_CURVE ( 'NONE', #2306, #2910, #16311, .T. ) ;
#7538 = ORIENTED_EDGE ( 'NONE', *, *, #20247, .F. ) ;
#7539 = CARTESIAN_POINT ( 'NONE',  ( 18.00000000000000000, -2.163824016901520184E-09, -6.871049999819685894 ) ) ;
#7540 = DIRECTION ( 'NONE',  ( -1.000000000000000000, 0.000000000000000000, 0.000000000000000000 ) ) ;
#7541 = VECTOR ( 'NONE', #18832, 1000.000000000000000 ) ;
#7542 = EDGE_LOOP ( 'NONE', ( #16685, #3780 ) ) ;
#7543 = AXIS2_PLACEMENT_3D ( 'NONE', #19481, #4966, #4861 ) ;
#7544 = DIRECTION ( 'NONE',  ( -1.000000000000000000, -0.000000000000000000, -0.000000000000000000 ) ) ;
#7545 = ORIENTED_EDGE ( 'NONE', *, *, #9952, .F. ) ;
#7546 = EDGE_CURVE ( 'NONE', #16499, #18514, #7317, .T. ) ;
#7547 = CARTESIAN_POINT ( 'NONE',  ( 6.929096493489625530, -2.870125743571142252, -8.462137499819693431 ) ) ;
#7548 = PLANE ( 'NONE',  #13124 ) ;
#7549 = CARTESIAN_POINT ( 'NONE',  ( -6.165580000000000283, 0.000000000000000000, 0.000000000000000000 ) ) ;
#7550 = ORIENTED_EDGE ( 'NONE', *, *, #9843, .F. ) ;
#7551 = CARTESIAN_POINT ( 'NONE',  ( 19.99999999999999645, -51.81019761368347787, 38.98425606966041101 ) ) ;
#7552 = VECTOR ( 'NONE', #19131, 1000.000000000000000 ) ;
#7553 = DIRECTION ( 'NONE',  ( -0.000000000000000000, 0.000000000000000000, -1.000000000000000000 ) ) ;
#7554 = CARTESIAN_POINT ( 'NONE',  ( -12.50000000000000533, 0.000000000000000000, 166.0000000000000000 ) ) ;
#7555 = CARTESIAN_POINT ( 'NONE',  ( -12.50000000000000533, 0.000000000000000000, 40.00000000000000000 ) ) ;
#7556 = AXIS2_PLACEMENT_3D ( 'NONE', #15584, #1079, #14118 ) ;
#7557 = CARTESIAN_POINT ( 'NONE',  ( 0.000000000000000000, 0.000000000000000000, 0.000000000000000000 ) ) ;
#7558 = AXIS2_PLACEMENT_3D ( 'NONE', #13606, #10650, #5749 ) ;
#7560 = ORIENTED_EDGE ( 'NONE', *, *, #18112, .T. ) ;
#7559 = VECTOR ( 'NONE', #8809, 1000.000000000000000 ) ;
#7561 = ADVANCED_FACE ( 'NONE', ( #9844 ), #17495, .F. ) ;
#7562 = ADVANCED_FACE ( 'NONE', ( #1900 ), #5281, .T. ) ;
#7563 = LINE ( 'NONE', #1537, #12722 ) ;
#7564 = LINE ( 'NONE', #5872, #15578 ) ;
#7565 = ORIENTED_EDGE ( 'NONE', *, *, #14542, .T. ) ;
#7566 = LINE ( 'NONE', #6182, #2160 ) ;
#7567 = DIRECTION ( 'NONE',  ( 1.000000000000000000, 0.000000000000000000, 0.000000000000000000 ) ) ;
#7568 = ORIENTED_EDGE ( 'NONE', *, *, #15695, .F. ) ;
#7569 = CARTESIAN_POINT ( 'NONE',  ( -6.888301784570738384, -16.62983158437509346, -20.87113749981968880 ) ) ;
#7570 = EDGE_CURVE ( 'NONE', #8121, #11513, #12118, .T. ) ;
#7571 = DIRECTION ( 'NONE',  ( 1.000000000000000000, 0.000000000000000000, 0.000000000000000000 ) ) ;
#7572 = DIRECTION ( 'NONE',  ( 0.000000000000000000, 0.000000000000000000, 1.000000000000000000 ) ) ;
#7573 = ORIENTED_EDGE ( 'NONE', *, *, #4933, .F. ) ;
#7574 = AXIS2_PLACEMENT_3D ( 'NONE', #17587, #4338, #4545 ) ;
#7575 = CIRCLE ( 'NONE', #11300, 72.00000000007199219 ) ;
#7576 = CARTESIAN_POINT ( 'NONE',  ( 7.500000000000004441, -8.788009009181406898E-15, -18.47619999999769647 ) ) ;
#7577 = ORIENTED_EDGE ( 'NONE', *, *, #19816, .T. ) ;
#7578 = CARTESIAN_POINT ( 'NONE',  ( -10.00000000000000000, 0.000000000000000000, 0.000000000000000000 ) ) ;
#7579 = ORIENTED_EDGE ( 'NONE', *, *, #15982, .F. ) ;
#7580 = CIRCLE ( 'NONE', #8236, 72.00000000007199219 ) ;
#7581 = VECTOR ( 'NONE', #5397, 1000.000000000000000 ) ;
#7582 = CIRCLE ( 'NONE', #16383, 27.60000000002759890 ) ;
#7583 = ADVANCED_FACE ( 'NONE', ( #6667 ), #6762, .T. ) ;
#7584 = CARTESIAN_POINT ( 'NONE',  ( 32.99516560860324432, -115.5366112665960259, 75.94268391876913427 ) ) ;
#7585 = DIRECTION ( 'NONE',  ( 0.000000000000000000, 1.000000000000000000, 0.000000000000000000 ) ) ;
#7586 = ITEM_DEFINED_TRANSFORMATION ( 'NONE', 'NONE', #5923,  #12461 ) ;
#7587 = AXIS2_PLACEMENT_3D ( 'NONE', #2477, #12014, #18480 ) ;
#7588 = CARTESIAN_POINT ( 'NONE',  ( 14.79893867722910450, -2.943691928843438443, 6.609823168841544749 ) ) ;
#7589 = VERTEX_POINT ( 'NONE', #13241 ) ;
#7590 = CARTESIAN_POINT ( 'NONE',  ( 19.99999999999999645, -58.44960523466222213, -28.06621538408651872 ) ) ;
#7591 = ORIENTED_EDGE ( 'NONE', *, *, #13412, .T. ) ;
#7592 = CIRCLE ( 'NONE', #10300, 72.00000000007199219 ) ;
#7593 = DIRECTION ( 'NONE',  ( 0.000000000000000000, 0.6310879443260539734, -0.7757112907044189098 ) ) ;
#7594 = CARTESIAN_POINT ( 'NONE',  ( 10.19618095414378622, 15.25966316918061239, 10.50629375018031020 ) ) ;
#7595 = VECTOR ( 'NONE', #7540, 1000.000000000000000 ) ;
#7596 = CARTESIAN_POINT ( 'NONE',  ( 6.929096494179677990, 2.870125741905210859, -19.06526249981969556 ) ) ;
#7597 = CARTESIAN_POINT ( 'NONE',  ( -7.500000000000000000, 0.000000000000000000, 46.00000000000000711 ) ) ;
#7598 = EDGE_LOOP ( 'NONE', ( #13936, #16162, #9913, #16785 ) ) ;
#7599 = DIRECTION ( 'NONE',  ( 0.000000000000000000, 0.000000000000000000, -1.000000000000000000 ) ) ;
#7600 = DIRECTION ( 'NONE',  ( -0.000000000000000000, -0.000000000000000000, -1.000000000000000000 ) ) ;
#7601 = ORIENTED_EDGE ( 'NONE', *, *, #2496, .F. ) ;
#7602 = CARTESIAN_POINT ( 'NONE',  ( 17.19937875120477955, -15.27427100821770800, -79.49209680402589129 ) ) ;
#7603 = EDGE_CURVE ( 'NONE', #254, #4449, #14779, .T. ) ;
#7604 = DIRECTION ( 'NONE',  ( -1.000000000000000000, 0.000000000000000000, 0.000000000000000000 ) ) ;
#7605 = CARTESIAN_POINT ( 'NONE',  ( 12.72792206288790773, 12.72792205982779912, -8.049174999819690868 ) ) ;
#7606 = EDGE_CURVE ( 'NONE', #65, #13495, #5293, .T. ) ;
#7607 = ORIENTED_EDGE ( 'NONE', *, *, #19855, .T. ) ;
#7608 = CARTESIAN_POINT ( 'NONE',  ( -5.303300859536636658, -5.303300858261589035, -8.676924999819688011 ) ) ;
#7609 = LINE ( 'NONE', #4220, #8176 ) ;
#7610 = FACE_BOUND ( 'NONE', #12126, .T. ) ;
#7611 = CARTESIAN_POINT ( 'NONE',  ( 2.500000000000000000, 2.357898499370433054, -1.951563910473907981E-15 ) ) ;
#7612 = DIRECTION ( 'NONE',  ( 1.760777620558074541E-30, -1.056873212472353686E-31, -1.000000000000000000 ) ) ;
#7613 = CARTESIAN_POINT ( 'NONE',  ( -18.00000000000000355, 2.163826221265759298E-09, -0.2539499998196921293 ) ) ;
#7614 = CARTESIAN_POINT ( 'NONE',  ( -1.491842756249033064, -7.499999999820668783, -18.98551874981968268 ) ) ;
#7615 = ORIENTED_EDGE ( 'NONE', *, *, #20832, .T. ) ;
#7616 = CARTESIAN_POINT ( 'NONE',  ( 19.99999999999999645, -46.01927912072559224, 45.67597560296373871 ) ) ;
#7617 = DIRECTION ( 'NONE',  ( 0.000000000000000000, 0.000000000000000000, 1.000000000000000000 ) ) ;
#7618 = CARTESIAN_POINT ( 'NONE',  ( -2.943691928843435779, -14.79893867722909917, 12.77298933151907612 ) ) ;
#7619 = B_SPLINE_CURVE_WITH_KNOTS ( 'NONE', 3,
 ( #17065, #7408, #7625, #12616 ),
 .UNSPECIFIED., .F., .F.,
 ( 4, 4 ),
 ( 2.797157557069881010E-17, 0.007433635558789152172 ),
 .UNSPECIFIED. ) ;
#7620 = CARTESIAN_POINT ( 'NONE',  ( 50.00000000000000000, -170.8299878242309546, 15.48896927112552824 ) ) ;
#7621 = VECTOR ( 'NONE', #19227, 1000.000000000000000 ) ;
#7622 = ORIENTED_EDGE ( 'NONE', *, *, #12066, .F. ) ;
#7623 = DIRECTION ( 'NONE',  ( 0.000000000000000000, 0.000000000000000000, -1.000000000000000000 ) ) ;
#7624 = CARTESIAN_POINT ( 'NONE',  ( 2.500000000000000000, 2.357898499370431722, -2.818925648462311528E-15 ) ) ;
#7625 = CARTESIAN_POINT ( 'NONE',  ( 30.14545621897691774, -45.03477164951879530, -71.38288848018790134 ) ) ;
#7626 = EDGE_LOOP ( 'NONE', ( #20449, #13200, #4691, #10653 ) ) ;
#7627 = CARTESIAN_POINT ( 'NONE',  ( 0.000000000000000000, 51.96384592647267908, -49.83732252579563493 ) ) ;
#7628 = ORIENTED_EDGE ( 'NONE', *, *, #6830, .F. ) ;
#7629 = CARTESIAN_POINT ( 'NONE',  ( 37.09297593336772536, -20.77527980508516592, -76.37819121560252711 ) ) ;
#7630 = DIRECTION ( 'NONE',  ( 0.000000000000000000, 0.000000000000000000, 1.000000000000000000 ) ) ;
#7631 = VERTEX_POINT ( 'NONE', #11645 ) ;
#7632 = VERTEX_POINT ( 'NONE', #3584 ) ;
#7633 = CARTESIAN_POINT ( 'NONE',  ( 39.62131026106984422, -122.1018714529781022, -80.10792010848122402 ) ) ;
#7634 = AXIS2_PLACEMENT_3D ( 'NONE', #7718, #9719, #19567 ) ;
#7635 = PRESENTATION_STYLE_ASSIGNMENT (( #3075 ) ) ;
#7636 = EDGE_CURVE ( 'NONE', #17663, #1747, #16815, .T. ) ;
#7637 = CARTESIAN_POINT ( 'NONE',  ( 0.000000000000000000, 63.48283426024899256, -33.96954156735303343 ) ) ;
#7638 = EDGE_CURVE ( 'NONE', #6274, #12091, #3278, .T. ) ;
#7639 = AXIS2_PLACEMENT_3D ( 'NONE', #20299, #3796, #17142 ) ;
#7640 = FILL_AREA_STYLE_COLOUR ( '', #10207 ) ;
#7641 = CARTESIAN_POINT ( 'NONE',  ( 6.929096493489624642, -2.870125743571141363, -27.31213749981969130 ) ) ;
#7642 = LINE ( 'NONE', #4137, #4762 ) ;
#7643 = LINE ( 'NONE', #2987, #18301 ) ;
#7644 = CARTESIAN_POINT ( 'NONE',  ( 2.500000000000000000, -1.178949249685214307, 2.042000000000001592 ) ) ;
#7645 = EDGE_CURVE ( 'NONE', #1438, #3529, #523, .T. ) ;
#7646 = ORIENTED_EDGE ( 'NONE', *, *, #1510, .T. ) ;
#7647 = FACE_OUTER_BOUND ( 'NONE', #1010, .T. ) ;
#7648 = ORIENTED_EDGE ( 'NONE', *, *, #12147, .F. ) ;
#7649 = CARTESIAN_POINT ( 'NONE',  ( 10.19618095047497874, -15.25966317163203279, -24.24839374981968732 ) ) ;
#7650 = CARTESIAN_POINT ( 'NONE',  ( 50.00000000000000000, -160.0000000000000000, 79.59486983196745769 ) ) ;
#7651 = ORIENTED_EDGE ( 'NONE', *, *, #12153, .T. ) ;
#7652 = CARTESIAN_POINT ( 'NONE',  ( 0.000000000000000000, 0.000000000000000000, -84.99999999999998579 ) ) ;
#7653 = CIRCLE ( 'NONE', #5616, 27.60000000002759890 ) ;
#7654 = ORIENTED_EDGE ( 'NONE', *, *, #20226, .F. ) ;
#7655 = AXIS2_PLACEMENT_3D ( 'NONE', #4413, #9296, #6319 ) ;
#7656 = DIRECTION ( 'NONE',  ( -0.000000000000000000, -0.000000000000000000, -1.000000000000000000 ) ) ;
#7657 = FACE_OUTER_BOUND ( 'NONE', #11930, .T. ) ;
#7658 = CARTESIAN_POINT ( 'NONE',  ( 19.99999999999999645, -0.9548212943360466776, -71.99366858485716136 ) ) ;
#7659 = VERTEX_POINT ( 'NONE', #8563 ) ;
#7660 = CARTESIAN_POINT ( 'NONE',  ( 30.00000000000000000, -99.99999999999998579, 54.09999999999999432 ) ) ;
#7661 = AXIS2_PLACEMENT_3D ( 'NONE', #20838, #354, #18163 ) ;
#7662 = CARTESIAN_POINT ( 'NONE',  ( 19.99999999999999645, 0.000000000000000000, 0.000000000000000000 ) ) ;
#7663 = CARTESIAN_POINT ( 'NONE',  ( 9.999999999999998224, 44.69367065308645692, 56.44887778834763026 ) ) ;
#7664 = FACE_OUTER_BOUND ( 'NONE', #18368, .T. ) ;
#7665 = EDGE_CURVE ( 'NONE', #2235, #3334, #10478, .T. ) ;
#7666 = CIRCLE ( 'NONE', #8016, 2.500000000000000444 ) ;
#7667 = AXIS2_PLACEMENT_3D ( 'NONE', #18315, #627, #11752 ) ;
#7668 = EDGE_CURVE ( 'NONE', #17731, #13498, #10385, .T. ) ;
#7669 = DIRECTION ( 'NONE',  ( 0.000000000000000000, -0.2697967711570115057, -0.9629172873478027972 ) ) ;
#7670 = ORIENTED_EDGE ( 'NONE', *, *, #1161, .F. ) ;
#7671 = AXIS2_PLACEMENT_3D ( 'NONE', #8244, #14720, #17996 ) ;
#7672 = AXIS2_PLACEMENT_3D ( 'NONE', #796, #5662, #17118 ) ;
#7673 = LINE ( 'NONE', #11070, #5579 ) ;
#7674 = PRESENTATION_LAYER_ASSIGNMENT (  '', '', ( #17505 ) ) ;
#7675 = ADVANCED_FACE ( 'NONE', ( #3784 ), #10373, .T. ) ;
#7676 = DIRECTION ( 'NONE',  ( -1.000000000000000000, -0.000000000000000000, -0.000000000000000000 ) ) ;
#7677 = EDGE_LOOP ( 'NONE', ( #3473, #18980, #6420 ) ) ;
#7678 = DIRECTION ( 'NONE',  ( -1.000000000000000000, 0.000000000000000000, 0.000000000000000000 ) ) ;
#7679 = CARTESIAN_POINT ( 'NONE',  ( 0.000000000000000000, 48.70996102988739551, -42.79495875147724604 ) ) ;
#7680 = EDGE_LOOP ( 'NONE', ( #16156, #17318, #6683, #13375, #11865, #20156, #332, #20677 ) ) ;
#7681 = CARTESIAN_POINT ( 'NONE',  ( 10.19618095414378800, 15.25966316918061416, -6.439106249819689154 ) ) ;
#7682 = VECTOR ( 'NONE', #20794, 1000.000000000000000 ) ;
#7683 = CARTESIAN_POINT ( 'NONE',  ( -39.99999999999999289, -40.00000000000000000, -120.0000000000000142 ) ) ;
#7684 = DIRECTION ( 'NONE',  ( -0.000000000000000000, -0.000000000000000000, -1.000000000000000000 ) ) ;
#7685 = VERTEX_POINT ( 'NONE', #18752 ) ;
#7686 = CARTESIAN_POINT ( 'NONE',  ( 19.99999999999999645, -48.70996102988709708, 42.79495875147758710 ) ) ;
#7687 = VECTOR ( 'NONE', #11850, 1000.000000000000000 ) ;
#7688 = ORIENTED_EDGE ( 'NONE', *, *, #5199, .F. ) ;
#7689 = CARTESIAN_POINT ( 'NONE',  ( -39.99999999999999289, -30.00000000000000000, -120.0000000000000142 ) ) ;
#7690 = VECTOR ( 'NONE', #4073, 1000.000000000000000 ) ;
#7691 = ADVANCED_FACE ( 'NONE', ( #19905 ), #5800, .F. ) ;
#7692 = VERTEX_POINT ( 'NONE', #15350 ) ;
#7693 = EDGE_CURVE ( 'NONE', #14024, #14670, #5381, .T. ) ;
#7694 = CIRCLE ( 'NONE', #2624, 21.50000000000000000 ) ;
#7695 = AXIS2_PLACEMENT_3D ( 'NONE', #13468, #13671, #16738 ) ;
#7696 = LINE ( 'NONE', #15853, #14159 ) ;
#7697 = ADVANCED_FACE ( 'NONE', ( #2317 ), #4221, .T. ) ;
#7698 = DIRECTION ( 'NONE',  ( -1.000000000000000000, 0.000000000000000000, 0.000000000000000000 ) ) ;
#7699 = CIRCLE ( 'NONE', #10068, 10.85999999999999410 ) ;
#7700 = CARTESIAN_POINT ( 'NONE',  ( -12.54593441562641054, 8.382925371439629458, -6.938614331158453830 ) ) ;
#7701 = ORIENTED_EDGE ( 'NONE', *, *, #4494, .T. ) ;
#7702 = LINE ( 'NONE', #9493, #9977 ) ;
#7703 = AXIS2_PLACEMENT_3D ( 'NONE', #17340, #20614, #1133 ) ;
#7704 = CARTESIAN_POINT ( 'NONE',  ( 19.99999999999999645, 45.48683723007212620, 46.78012013466234720 ) ) ;
#7705 = ORIENTED_EDGE ( 'NONE', *, *, #17169, .T. ) ;
#7706 = CARTESIAN_POINT ( 'NONE',  ( 13.11093970363753769, -17.09443977129685521, 78.35293316767238991 ) ) ;
#7707 = CIRCLE ( 'NONE', #8703, 80.00000000000000000 ) ;
#7708 = CARTESIAN_POINT ( 'NONE',  ( -6.888301784570736608, -16.62983158437509346, 14.92426250018031020 ) ) ;
#7709 = AXIS2_PLACEMENT_3D ( 'NONE', #18817, #10767, #17228 ) ;
#7710 = CARTESIAN_POINT ( 'NONE',  ( 8.899999999999890221, -10.82531754730554496, 126.0000000000000000 ) ) ;
#7711 = CARTESIAN_POINT ( 'NONE',  ( 0.000000000000000000, -2.357898499370432166, 3.035766082959412415E-15 ) ) ;
#7712 = VERTEX_POINT ( 'NONE', #16730 ) ;
#7713 = CARTESIAN_POINT ( 'NONE',  ( 6.250000000000054179, 10.82531754730546147, 43.00000000000000000 ) ) ;
#7714 = CARTESIAN_POINT ( 'NONE',  ( -9.850000000000012079, 0.000000000000000000, 43.00000000000000000 ) ) ;
#7715 = AXIS2_PLACEMENT_3D ( 'NONE', #19850, #2048, #18262 ) ;
#7716 = ORIENTED_EDGE ( 'NONE', *, *, #5865, .T. ) ;
#7717 = DIRECTION ( 'NONE',  ( 1.000000000000000000, 0.000000000000000000, 0.000000000000000000 ) ) ;
#7718 = CARTESIAN_POINT ( 'NONE',  ( 0.000000000000000000, -48.70996102988652154, -42.79495875147824790 ) ) ;
#7719 = CARTESIAN_POINT ( 'NONE',  ( 10.19618095414378622, 15.25966316918061239, -17.76870624981969371 ) ) ;
#7720 = CONICAL_SURFACE ( 'NONE', #6347, 4.000000000000000000, 1.047197551196595855 ) ;
#7721 = VERTEX_POINT ( 'NONE', #15460 ) ;
#7722 = DIRECTION ( 'NONE',  ( -0.000000000000000000, -1.000000000000000000, -0.000000000000000000 ) ) ;
#7723 = FACE_BOUND ( 'NONE', #11819, .T. ) ;
#7724 = DIRECTION ( 'NONE',  ( 0.000000000000000000, 0.000000000000000000, -1.000000000000000000 ) ) ;
#7725 = CARTESIAN_POINT ( 'NONE',  ( 2.500000000000000000, -1.178949249685213863, 2.042000000000002924 ) ) ;
#7726 = DIRECTION ( 'NONE',  ( 0.9237280213470682178, 0.3830490080632378835, 1.243481486083094649E-31 ) ) ;
#7727 = CARTESIAN_POINT ( 'NONE',  ( -2.163827323447878648E-09, -18.00000000000000355, -2.610199999819692973 ) ) ;
#7728 = CARTESIAN_POINT ( 'NONE',  ( 2.678494666091051357, 3.072372537026354156, -0.03421028094653023183 ) ) ;
#7729 = VERTEX_POINT ( 'NONE', #18540 ) ;
#7730 = DIRECTION ( 'NONE',  ( 0.000000000000000000, -0.5195839500354404450, 0.8544194045464844622 ) ) ;
#7731 = CARTESIAN_POINT ( 'NONE',  ( -10.46442989202483709, 10.46442989454075168, 16.01283308151908003 ) ) ;
#7732 = EDGE_CURVE ( 'NONE', #16753, #2149, #4294, .T. ) ;
#7733 = EDGE_LOOP ( 'NONE', ( #14127, #10474, #9065, #18002 ) ) ;
#7734 = DIRECTION ( 'NONE',  ( 0.000000000000000000, 0.000000000000000000, 1.000000000000000000 ) ) ;
#7735 = CARTESIAN_POINT ( 'NONE',  ( 3.580422614997668340, 17.99999999956958519, -16.45316874981969235 ) ) ;
#7736 = DIRECTION ( 'NONE',  ( 0.000000000000000000, 0.000000000000000000, -1.000000000000000000 ) ) ;
#7737 = ORIENTED_EDGE ( 'NONE', *, *, #9219, .T. ) ;
#7738 = CARTESIAN_POINT ( 'NONE',  ( 19.99999999999999645, -64.44931368725528387, 10.18420179740584608 ) ) ;
#7739 = ORIENTED_EDGE ( 'NONE', *, *, #5210, .F. ) ;
#7740 = CARTESIAN_POINT ( 'NONE',  ( -24.99999999999999289, -85.00000000000000000, -1.040949779275250179E-14 ) ) ;
#7741 = DIRECTION ( 'NONE',  ( -1.000000000000000000, 0.000000000000000000, 0.000000000000000000 ) ) ;
#7742 = EDGE_LOOP ( 'NONE', ( #569, #20791, #1445, #6571 ) ) ;
#7744 = ORIENTED_EDGE ( 'NONE', *, *, #20074, .F. ) ;
#7743 = B_SPLINE_CURVE_WITH_KNOTS ( 'NONE', 3,
 ( #20216, #15140, #12164, #7283, #8989, #5693 ),
 .UNSPECIFIED., .F., .F.,
 ( 4, 2, 4 ),
 ( 0.000000000000000000, 0.003996741055817027918, 0.007993482111634055837 ),
 .UNSPECIFIED. ) ;
#7745 = DIRECTION ( 'NONE',  ( 0.000000000000000000, -1.000000000000000000, 0.000000000000000000 ) ) ;
#7746 = FACE_OUTER_BOUND ( 'NONE', #20510, .T. ) ;
#7747 = LINE ( 'NONE', #6258, #3758 ) ;
#7748 = CARTESIAN_POINT ( 'NONE',  ( 7.902369976724399336, -7.902369978624331104, -1.179265249352571931 ) ) ;
#7749 = CARTESIAN_POINT ( 'NONE',  ( -9.015947181032828388E-10, -7.500000000000000888, -16.11994999981969556 ) ) ;
#7750 = ADVANCED_FACE ( 'NONE', ( #2209 ), #15239, .T. ) ;
#7751 = DIRECTION ( 'NONE',  ( 0.000000000000000000, 0.000000000000000000, 1.000000000000000000 ) ) ;
#7752 = DIRECTION ( 'NONE',  ( 0.000000000000000000, 0.000000000000000000, -1.000000000000000000 ) ) ;
#7753 = CARTESIAN_POINT ( 'NONE',  ( 0.000000000000000000, 0.000000000000000000, 84.99999999999998579 ) ) ;
#7754 = ORIENTED_EDGE ( 'NONE', *, *, #16966, .F. ) ;
#7755 = DIRECTION ( 'NONE',  ( 1.000000000000000000, 0.000000000000000000, 0.000000000000000000 ) ) ;
#7756 = VERTEX_POINT ( 'NONE', #15042 ) ;
#7757 = CARTESIAN_POINT ( 'NONE',  ( 18.00000000043041126, 3.580422610670019434, -16.59058124981968874 ) ) ;
#7758 = DIRECTION ( 'NONE',  ( 0.000000000000000000, 0.000000000000000000, 1.000000000000000000 ) ) ;
#7759 = ORIENTED_EDGE ( 'NONE', *, *, #8645, .F. ) ;
#7760 = ADVANCED_FACE ( 'NONE', ( #6969 ), #17847, .F. ) ;
#7761 = CARTESIAN_POINT ( 'NONE',  ( 0.000000000000000000, 42.42902769288603082, -49.02903636734153281 ) ) ;
#7762 = EDGE_LOOP ( 'NONE', ( #2665, #16982, #14718, #6555 ) ) ;
#7763 = CARTESIAN_POINT ( 'NONE',  ( -1.491842756249031954, -7.499999999820663454, -6.400418749819693609 ) ) ;
#7764 = CARTESIAN_POINT ( 'NONE',  ( 4.924999999999924327, -8.530350227276771946, -40.00000000000000000 ) ) ;
#7765 = CARTESIAN_POINT ( 'NONE',  ( 9.015937996181835182E-10, 7.500000000000002665, -1.982449999819692943 ) ) ;
#7766 = VERTEX_POINT ( 'NONE', #13552 ) ;
#7767 = CARTESIAN_POINT ( 'NONE',  ( 0.000000000000000000, 0.000000000000000000, 43.00000000000000000 ) ) ;
#7768 = CYLINDRICAL_SURFACE ( 'NONE', #1911, 2.649999999999999467 ) ;
#7769 = CARTESIAN_POINT ( 'NONE',  ( 17.99999999956957808, -3.580422614997675446, -25.42651874981969229 ) ) ;
#7770 = DIRECTION ( 'NONE',  ( -1.000000000000000000, 0.000000000000000000, 0.000000000000000000 ) ) ;
#7771 = CARTESIAN_POINT ( 'NONE',  ( -1.491842756249031954, -7.499999999820663454, 12.44958125018030870 ) ) ;
#7772 = ORIENTED_EDGE ( 'NONE', *, *, #3117, .T. ) ;
#7773 = CARTESIAN_POINT ( 'NONE',  ( -31.35784117651625635, 26.35784117651607872, -130.0000000000000000 ) ) ;
#7774 = DIRECTION ( 'NONE',  ( 1.000000000000000000, 0.000000000000000000, 0.000000000000000000 ) ) ;
#7775 = ORIENTED_EDGE ( 'NONE', *, *, #9754, .T. ) ;
#7776 = DIRECTION ( 'NONE',  ( -1.000000000000000000, -0.000000000000000000, 0.000000000000000000 ) ) ;
#7777 = CARTESIAN_POINT ( 'NONE',  ( -6.929096493489632635, 2.870125743571140919, -6.909737499819684992 ) ) ;
#7778 = ADVANCED_FACE ( 'NONE', ( #5695 ), #8991, .T. ) ;
#7779 = ORIENTED_EDGE ( 'NONE', *, *, #1446, .F. ) ;
#7780 = CARTESIAN_POINT ( 'NONE',  ( -10.19618095047498052, 15.25966317163203101, -8.206293749819685956 ) ) ;
#7781 = CARTESIAN_POINT ( 'NONE',  ( -6.999999999999995559, 4.546351088565595293E-15, 0.000000000000000000 ) ) ;
#7782 = DIRECTION ( 'NONE',  ( 1.000000000000000000, 0.000000000000000000, 0.000000000000000000 ) ) ;
#7783 = ORIENTED_EDGE ( 'NONE', *, *, #18170, .T. ) ;
#7784 = EDGE_CURVE ( 'NONE', #7685, #20241, #398, .T. ) ;
#7785 = DIRECTION ( 'NONE',  ( -1.202124453834178598E-10, -1.000000000000000000, 1.727264247904875625E-25 ) ) ;
#7786 = VERTEX_POINT ( 'NONE', #7393 ) ;
#7787 = FACE_OUTER_BOUND ( 'NONE', #19741, .T. ) ;
#7788 = ADVANCED_FACE ( 'NONE', ( #12069, #13869 ), #20316, .F. ) ;
#7789 = VERTEX_POINT ( 'NONE', #10799 ) ;
#7790 = ADVANCED_FACE ( 'NONE', ( #10999 ), #13979, .T. ) ;
#7791 = DIRECTION ( 'NONE',  ( 0.000000000000000000, 0.000000000000000000, 1.000000000000000000 ) ) ;
#7792 = DIRECTION ( 'NONE',  ( 1.000000000000000000, -0.000000000000000000, -0.000000000000000000 ) ) ;
#7793 = AXIS2_PLACEMENT_3D ( 'NONE', #6129, #11008, #12199 ) ;
#7794 = CARTESIAN_POINT ( 'NONE',  ( -10.46442989202484242, 10.46442989454075700, -16.06908308115845685 ) ) ;
#7795 = ORIENTED_EDGE ( 'NONE', *, *, #16233, .T. ) ;
#7796 = CARTESIAN_POINT ( 'NONE',  ( -2.870125743571141808, -6.929096493489625530, -15.53088749981969663 ) ) ;
#7797 = DIRECTION ( 'NONE',  ( -1.000000000000000000, -0.000000000000000000, -0.000000000000000000 ) ) ;
#7798 = ORIENTED_EDGE ( 'NONE', *, *, #6089, .F. ) ;
#7799 = CARTESIAN_POINT ( 'NONE',  ( 5.636490946615987596, -20.76011204682435718, 76.39151275260617524 ) ) ;
#7800 = ADVANCED_FACE ( 'NONE', ( #4333, #2841, #7610, #15771 ), #9308, .T. ) ;
#7801 = LINE ( 'NONE', #9497, #2414 ) ;
#7802 = DIRECTION ( 'NONE',  ( 0.000000000000000000, 0.000000000000000000, 1.000000000000000000 ) ) ;
#7803 = EDGE_CURVE ( 'NONE', #19780, #14868, #8180, .T. ) ;
#7804 = ORIENTED_EDGE ( 'NONE', *, *, #10571, .F. ) ;
#7805 = ADVANCED_FACE ( 'NONE', ( #15875 ), #4428, .T. ) ;
#7806 = DIRECTION ( 'NONE',  ( -1.000000000000000000, -0.000000000000000000, 0.000000000000000000 ) ) ;
#7807 = CARTESIAN_POINT ( 'NONE',  ( -2.500000000000002220, 0.000000000000000000, -5.574599999999999334 ) ) ;
#7808 = AXIS2_PLACEMENT_3D ( 'NONE', #19114, #2682, #2889 ) ;
#7809 = ORIENTED_EDGE ( 'NONE', *, *, #49, .T. ) ;
#7810 = CARTESIAN_POINT ( 'NONE',  ( 50.00000000000000000, 36.35083268962917202, 90.00000000000000000 ) ) ;
#7811 = CARTESIAN_POINT ( 'NONE',  ( 0.000000000000000000, 67.51707036274413554, 25.00890260772400708 ) ) ;
#7812 = EDGE_CURVE ( 'NONE', #19863, #10676, #2733, .T. ) ;
#7813 = CARTESIAN_POINT ( 'NONE',  ( -6.888301784570736608, -16.62983158437509346, -13.35073749981969371 ) ) ;
#7814 = ORIENTED_EDGE ( 'NONE', *, *, #5389, .T. ) ;
#7815 = CARTESIAN_POINT ( 'NONE',  ( 0.000000000000000000, 0.000000000000000000, -120.0000000000000142 ) ) ;
#7816 =( NAMED_UNIT ( * ) PLANE_ANGLE_UNIT ( ) SI_UNIT ( $, .RADIAN. ) );
#7817 = DIRECTION ( 'NONE',  ( -1.000000000000000000, 0.000000000000000000, 0.000000000000000000 ) ) ;
#7818 = CARTESIAN_POINT ( 'NONE',  ( 41.41808208302015970, -123.1392381480534226, 87.79662768828310959 ) ) ;
#7819 = DIRECTION ( 'NONE',  ( -1.000000000000000000, 0.000000000000000000, -6.982962677686266711E-15 ) ) ;
#7820 = CARTESIAN_POINT ( 'NONE',  ( -6.888301780572502864, 16.62983158603122646, 10.93823750018031049 ) ) ;
#7821 = CARTESIAN_POINT ( 'NONE',  ( 1.491842754445843688, -7.500000000179346316, -19.57458124981968695 ) ) ;
#7822 = AXIS2_PLACEMENT_3D ( 'NONE', #16952, #2435, #15790 ) ;
#7823 = VERTEX_POINT ( 'NONE', #17476 ) ;
#7824 = DIRECTION ( 'NONE',  ( 0.000000000000000000, 1.000000000000000000, 1.040834085586084454E-15 ) ) ;
#7825 = ADVANCED_FACE ( 'NONE', ( #9420 ), #1273, .T. ) ;
#7826 = CARTESIAN_POINT ( 'NONE',  ( 13.67243654642774686, -5.663308650141536837, 10.71127058151907718 ) ) ;
#7827 = CARTESIAN_POINT ( 'NONE',  ( 19.99999999999999645, 54.08351995568706627, 35.76369202524519864 ) ) ;
#7828 = VERTEX_POINT ( 'NONE', #1162 ) ;
#7829 = CARTESIAN_POINT ( 'NONE',  ( 0.000000000000000000, 0.000000000000000000, 0.000000000000000000 ) ) ;
#7830 = CARTESIAN_POINT ( 'NONE',  ( 15.25966316918061416, -10.19618095414378622, -22.93285624981968951 ) ) ;
#7831 = CARTESIAN_POINT ( 'NONE',  ( 8.500000000000000000, 0.000000000000000000, 81.99999999999998579 ) ) ;
#7832 = VERTEX_POINT ( 'NONE', #14197 ) ;
#7833 = AXIS2_PLACEMENT_3D ( 'NONE', #2320, #7182, #20003 ) ;
#7834 = PLANE ( 'NONE',  #8873 ) ;
#7835 = AXIS2_PLACEMENT_3D ( 'NONE', #6101, #7479, #14390 ) ;
#7836 = EDGE_LOOP ( 'NONE', ( #11884, #20659, #5278, #16232 ) ) ;
#7837 = DIRECTION ( 'NONE',  ( 0.000000000000000000, -0.1361666490962539222, 0.9906859460363298675 ) ) ;
#7838 = FACE_OUTER_BOUND ( 'NONE', #20308, .T. ) ;
#7839 = ORIENTED_EDGE ( 'NONE', *, *, #6020, .T. ) ;
#7840 = AXIS2_PLACEMENT_3D ( 'NONE', #19792, #7279, #13759 ) ;
#7841 = VERTEX_POINT ( 'NONE', #14295 ) ;
#7842 = LINE ( 'NONE', #14324, #14464 ) ;
#7843 = EDGE_CURVE ( 'NONE', #2697, #17420, #2095, .T. ) ;
#7844 = SURFACE_STYLE_FILL_AREA ( #16118 ) ;
#7845 = AXIS2_PLACEMENT_3D ( 'NONE', #6024, #13767, #15551 ) ;
#7846 = CARTESIAN_POINT ( 'NONE',  ( 39.99999999999999289, -122.3205080756887639, -86.97287527660684248 ) ) ;
#7847 = DIRECTION ( 'NONE',  ( 0.000000000000000000, 0.000000000000000000, 1.000000000000000000 ) ) ;
#7848 = CARTESIAN_POINT ( 'NONE',  ( 6.330490858644141738, 9.474249097082498849, -3.830046499352573797 ) ) ;
#7849 = AXIS2_PLACEMENT_3D ( 'NONE', #12790, #8002, #14482 ) ;
#7850 = VECTOR ( 'NONE', #12783, 1000.000000000000000 ) ;
#7851 = CARTESIAN_POINT ( 'NONE',  ( -4.248408730893245000, -6.358192987158590270, -24.66135624981969698 ) ) ;
#7852 = DIRECTION ( 'NONE',  ( -1.000000000000000000, 0.000000000000000000, 0.000000000000000000 ) ) ;
#7853 = CIRCLE ( 'NONE', #6824, 2.700000000000000622 ) ;
#7854 = CARTESIAN_POINT ( 'NONE',  ( 19.99999999999999645, 20.60847369612982405, 61.90898814327722732 ) ) ;
#7855 = CARTESIAN_POINT ( 'NONE',  ( 24.99999999999999645, -99.99999999999998579, 54.09999999999999432 ) ) ;
#7856 = ORIENTED_EDGE ( 'NONE', *, *, #2345, .F. ) ;
#7857 = FACE_OUTER_BOUND ( 'NONE', #16580, .T. ) ;
#7858 = ORIENTED_EDGE ( 'NONE', *, *, #15727, .F. ) ;
#7859 = CARTESIAN_POINT ( 'NONE',  ( -18.00000000043041126, -3.580422610670022543, -11.87808124981968838 ) ) ;
#7860 = DIRECTION ( 'NONE',  ( -1.000000000000000000, 0.000000000000000000, 0.000000000000000000 ) ) ;
#7861 = ORIENTED_EDGE ( 'NONE', *, *, #14807, .F. ) ;
#7862 = DIRECTION ( 'NONE',  ( 0.000000000000000000, 0.000000000000000000, 1.000000000000000000 ) ) ;
#7863 = ORIENTED_EDGE ( 'NONE', *, *, #19224, .T. ) ;
#7864 = DIRECTION ( 'NONE',  ( -1.000000000000000000, 0.000000000000000000, -0.000000000000000000 ) ) ;
#7865 = CARTESIAN_POINT ( 'NONE',  ( 50.00000000000000000, 230.0000000000000000, 84.99999999999998579 ) ) ;
#7866 = CARTESIAN_POINT ( 'NONE',  ( 8.899999999999900879, -10.82531754730554496, 43.00000000000000000 ) ) ;
#7867 = VERTEX_POINT ( 'NONE', #14088 ) ;
#7868 = DIRECTION ( 'NONE',  ( -1.000000000000000000, 0.000000000000000000, -0.000000000000000000 ) ) ;
#7869 = AXIS2_PLACEMENT_3D ( 'NONE', #2734, #2416, #15351 ) ;
#7870 = AXIS2_PLACEMENT_3D ( 'NONE', #3489, #10282, #636 ) ;
#7871 = EDGE_CURVE ( 'NONE', #4085, #4757, #6818, .T. ) ;
#7872 = CLOSED_SHELL ( 'NONE', ( #15585, #13504, #4071, #16328, #15702, #13043, #4577, #1011, #14306, #14016, #20326, #5585, #8284, #2762, #12749, #9733, #509, #19068, #4262, #20002, #12008, #10242 ) ) ;
#7873 = DIRECTION ( 'NONE',  ( 0.000000000000000000, 0.000000000000000000, -1.000000000000000000 ) ) ;
#7874 = FACE_OUTER_BOUND ( 'NONE', #14113, .T. ) ;
#7875 = CARTESIAN_POINT ( 'NONE',  ( 52.00000000000000000, -39.99999999999999289, 5.000000000000000000 ) ) ;
#7876 = EDGE_LOOP ( 'NONE', ( #1819, #4800, #13756, #13839 ) ) ;
#7877 = CARTESIAN_POINT ( 'NONE',  ( 0.000000000000000000, 1.178949249685218525, 2.041999999999999371 ) ) ;
#7878 = CARTESIAN_POINT ( 'NONE',  ( 23.13963350654227824, -26.35784117651622793, -130.0000000000000000 ) ) ;
#7879 = ORIENTED_EDGE ( 'NONE', *, *, #18675, .F. ) ;
#7880 = DIRECTION ( 'NONE',  ( -0.000000000000000000, 1.000000000000000000, 1.224646799147353207E-16 ) ) ;
#7881 = CARTESIAN_POINT ( 'NONE',  ( 19.99999999999999645, -46.01927912072495275, -45.67597560296436399 ) ) ;
#7882 = CIRCLE ( 'NONE', #20041, 65.24900000006525147 ) ;
#7883 = CIRCLE ( 'NONE', #16010, 27.60000000002759890 ) ;
#7884 = ORIENTED_EDGE ( 'NONE', *, *, #18932, .T. ) ;
#7885 = CARTESIAN_POINT ( 'NONE',  ( 24.74873734152916072, 24.74873734152916072, -120.0000000000000142 ) ) ;
#7886 = PRESENTATION_LAYER_ASSIGNMENT (  '', '', ( #2468 ) ) ;
#7887 = DIRECTION ( 'NONE',  ( -1.000000000000000000, 0.000000000000000000, -0.000000000000000000 ) ) ;
#7888 = DIRECTION ( 'NONE',  ( -0.000000000000000000, -0.000000000000000000, 1.000000000000000000 ) ) ;
#7889 = EDGE_CURVE ( 'NONE', #10195, #18098, #4810, .T. ) ;
#7890 = ORIENTED_EDGE ( 'NONE', *, *, #1711, .F. ) ;
#7891 = DIRECTION ( 'NONE',  ( 0.000000000000000000, -0.5195839500354404450, 0.8544194045464843512 ) ) ;
#7892 = ORIENTED_EDGE ( 'NONE', *, *, #11204, .F. ) ;
#7893 = DIRECTION ( 'NONE',  ( -1.000000000000000000, -0.000000000000000000, -0.000000000000000000 ) ) ;
#7894 = ORIENTED_EDGE ( 'NONE', *, *, #5592, .F. ) ;
#7895 = VECTOR ( 'NONE', #19928, 1000.000000000000000 ) ;
#7896 = DIRECTION ( 'NONE',  ( 0.000000000000000000, 0.000000000000000000, -1.000000000000000000 ) ) ;
#7897 = AXIS2_PLACEMENT_3D ( 'NONE', #19144, #18934, #17657 ) ;
#7898 = AXIS2_PLACEMENT_3D ( 'NONE', #11891, #8926, #12004 ) ;
#7899 = CARTESIAN_POINT ( 'NONE',  ( -9.850000000000006750, 0.000000000000000000, 40.00000000000000000 ) ) ;
#7900 = APPLICATION_CONTEXT ( 'automotive_design' ) ;
#7901 = ITEM_DEFINED_TRANSFORMATION ( 'NONE', 'NONE', #4909,  #12461 ) ;
#7902 = CARTESIAN_POINT ( 'NONE',  ( -14.79893867722910628, 2.943691928843437111, -16.95267683115846324 ) ) ;
#7903 = EDGE_CURVE ( 'NONE', #20609, #125, #20007, .T. ) ;
#7904 = ORIENTED_EDGE ( 'NONE', *, *, #11314, .T. ) ;
#7905 = CYLINDRICAL_SURFACE ( 'NONE', #15070, 27.60000000002759535 ) ;
#7906 = ADVANCED_BREP_SHAPE_REPRESENTATION ( '', ( #17220, #12461 ), #5607 ) ;
#7907 = EDGE_CURVE ( 'NONE', #8783, #18257, #7251, .T. ) ;
#7908 = FACE_BOUND ( 'NONE', #13315, .T. ) ;
#7909 = VERTEX_POINT ( 'NONE', #12358 ) ;
#7910 = CARTESIAN_POINT ( 'NONE',  ( -6.929096494179678878, -2.870125741905209971, -23.77776249981969769 ) ) ;
#7911 = VECTOR ( 'NONE', #19267, 1000.000000000000000 ) ;
#7912 = CARTESIAN_POINT ( 'NONE',  ( 24.99999999999999645, -30.00000000000000711, -1.040949779275250179E-14 ) ) ;
#7913 = ADVANCED_FACE ( 'NONE', ( #3862 ), #16801, .T. ) ;
#7914 = CIRCLE ( 'NONE', #14695, 2.649999999999999467 ) ;
#7915 = VECTOR ( 'NONE', #6060, 1000.000000000000000 ) ;
#7916 = ORIENTED_EDGE ( 'NONE', *, *, #13741, .F. ) ;
#7917 = CARTESIAN_POINT ( 'NONE',  ( -4.000000000000000000, 0.7862748000878058141, -0.03447227762756577968 ) ) ;
#7918 = DIRECTION ( 'NONE',  ( 1.000000000000000000, 0.000000000000000000, 0.000000000000000000 ) ) ;
#7919 = EDGE_LOOP ( 'NONE', ( #3739, #12021 ) ) ;
#7920 = DIRECTION ( 'NONE',  ( 1.000000000000000000, -0.000000000000000000, -0.000000000000000000 ) ) ;
#7921 = DIRECTION ( 'NONE',  ( 0.000000000000000000, 0.000000000000000000, 1.000000000000000000 ) ) ;
#7922 = PLANE ( 'NONE',  #20741 ) ;
#7923 = CONICAL_SURFACE ( 'NONE', #13341, 2.055000000000000160, 0.7853981633974639331 ) ;
#7924 = ORIENTED_EDGE ( 'NONE', *, *, #9370, .T. ) ;
#7925 = DIRECTION ( 'NONE',  ( 0.000000000000000000, -0.5195839500354229035, -0.8544194045464950094 ) ) ;
#7926 = CIRCLE ( 'NONE', #6899, 7.500000000000000888 ) ;
#7927 = EDGE_CURVE ( 'NONE', #14524, #11622, #4458, .T. ) ;
#7928 = SURFACE_STYLE_USAGE ( .BOTH. , #16471 ) ;
#7929 = DIRECTION ( 'NONE',  ( -0.000000000000000000, -0.000000000000000000, 1.000000000000000000 ) ) ;
#7930 = DIRECTION ( 'NONE',  ( 1.000000000000000000, 0.000000000000000000, 0.000000000000000000 ) ) ;
#7931 = CARTESIAN_POINT ( 'NONE',  ( 18.00000000000000355, -2.163824016901520597E-09, -14.39144999981969342 ) ) ;
#7932 = CIRCLE ( 'NONE', #9948, 65.24900000006523726 ) ;
#7933 = ADVANCED_FACE ( 'NONE', ( #12241 ), #735, .T. ) ;
#7934 = CIRCLE ( 'NONE', #8256, 14.49999999999999467 ) ;
#7935 = ADVANCED_FACE ( 'NONE', ( #17123 ), #4187, .F. ) ;
#7936 = CARTESIAN_POINT ( 'NONE',  ( -2.870125743571144028, -6.929096493489630859, -18.69098749981968410 ) ) ;
#7937 = PLANE ( 'NONE',  #1954 ) ;
#7938 = CARTESIAN_POINT ( 'NONE',  ( 14.79893867758296544, -1.779016607511491977E-09, -8.727791918480926725 ) ) ;
#7939 = DIRECTION ( 'NONE',  ( -1.000000000000000000, 0.000000000000000000, 0.000000000000000000 ) ) ;
#7940 = EDGE_CURVE ( 'NONE', #1354, #9669, #733, .T. ) ;
#7941 = VECTOR ( 'NONE', #448, 1000.000000000000114 ) ;
#7942 = ORIENTED_EDGE ( 'NONE', *, *, #12088, .T. ) ;
#7943 = LINE ( 'NONE', #11221, #11909 ) ;
#7944 = DIRECTION ( 'NONE',  ( 0.000000000000000000, 0.000000000000000000, 1.000000000000000000 ) ) ;
#7945 = DIRECTION ( 'NONE',  ( -1.000000000000000000, -0.000000000000000000, 0.000000000000000000 ) ) ;
#7946 = ORIENTED_EDGE ( 'NONE', *, *, #2872, .T. ) ;
#7947 = DIRECTION ( 'NONE',  ( 0.000000000000000000, 0.000000000000000000, -1.000000000000000000 ) ) ;
#7948 = EDGE_LOOP ( 'NONE', ( #2686, #5056, #183, #12325, #12620, #19594, #16025, #3226 ) ) ;
#7949 = AXIS2_PLACEMENT_3D ( 'NONE', #13257, #3088, #3491 ) ;
#7950 = FACE_BOUND ( 'NONE', #16680, .T. ) ;
#7951 = DIRECTION ( 'NONE',  ( 0.000000000000000000, 0.3984010898462422290, -0.9172113015054527141 ) ) ;
#7952 = ORIENTED_EDGE ( 'NONE', *, *, #15009, .T. ) ;
#7953 = ADVANCED_FACE ( 'NONE', ( #15211 ), #8958, .T. ) ;
#7954 = EDGE_LOOP ( 'NONE', ( #5095, #303, #6015, #11317, #18027 ) ) ;
#7955 = CARTESIAN_POINT ( 'NONE',  ( 5.200000000000002842, 0.000000000000000000, -2.700000000000000622 ) ) ;
#7956 = EDGE_CURVE ( 'NONE', #20282, #4158, #690, .T. ) ;
#7957 = EDGE_CURVE ( 'NONE', #2701, #12906, #912, .T. ) ;
#7958 = SURFACE_SIDE_STYLE ('',( #17818 ) ) ;
#7959 = STYLED_ITEM ( 'NONE', ( #8878 ), #14262 ) ;
#7960 = CYLINDRICAL_SURFACE ( 'NONE', #8233, 23.00000000000000000 ) ;
#7961 = EDGE_CURVE ( 'NONE', #12996, #9191, #2385, .T. ) ;
#7962 =( NAMED_UNIT ( * ) PLANE_ANGLE_UNIT ( ) SI_UNIT ( $, .RADIAN. ) );
#7963 = CARTESIAN_POINT ( 'NONE',  ( 6.330490858644141738, 9.474249097082498849, -13.25504649935257895 ) ) ;
#7964 = CARTESIAN_POINT ( 'NONE',  ( 7.902369978624323110, 7.902369976724394895, 17.61676524971320390 ) ) ;
#7965 = DIRECTION ( 'NONE',  ( 0.000000000000000000, -0.9790840876823249106, 0.2034560130526240906 ) ) ;
#7966 = FACE_OUTER_BOUND ( 'NONE', #14045, .T. ) ;
#7967 = CYLINDRICAL_SURFACE ( 'NONE', #10706, 14.49999999999999467 ) ;
#7968 = ORIENTED_EDGE ( 'NONE', *, *, #20864, .T. ) ;
#7969 = CARTESIAN_POINT ( 'NONE',  ( -2.099999999999999645, 2.571758278209440971E-16, -5.599999999999999645 ) ) ;
#7970 = ORIENTED_EDGE ( 'NONE', *, *, #2738, .F. ) ;
#7971 = CARTESIAN_POINT ( 'NONE',  ( 16.62983158437509346, -6.888301784570739272, -6.281987499819688736 ) ) ;
#7972 = CARTESIAN_POINT ( 'NONE',  ( 0.000000000000000000, -45.48683723007244595, 46.78012013466202035 ) ) ;
#7973 = PRODUCT_DEFINITION_FORMATION_WITH_SPECIFIED_SOURCE ( 'ANY', '', #13917, .NOT_KNOWN. ) ;
#7974 = VERTEX_POINT ( 'NONE', #5446 ) ;
#7975 = CARTESIAN_POINT ( 'NONE',  ( -2.681483223904239210, 3.070647092368425479, 2.604296331179000749E-15 ) ) ;
#7976 = ORIENTED_EDGE ( 'NONE', *, *, #7299, .F. ) ;
#7977 = CARTESIAN_POINT ( 'NONE',  ( 5.303300858261583706, -5.303300859536632217, -7.873074999819692721 ) ) ;
#7978 = LINE ( 'NONE', #12654, #12805 ) ;
#7979 = DIRECTION ( 'NONE',  ( 1.000000000000000000, 1.836909530733573776E-16, 0.000000000000000000 ) ) ;
#7980 = ORIENTED_EDGE ( 'NONE', *, *, #6615, .T. ) ;
#7981 = CARTESIAN_POINT ( 'NONE',  ( 0.000000000000000000, 20.34307325858884141, -69.06634035770285607 ) ) ;
#7982 = VECTOR ( 'NONE', #18990, 1000.000000000000114 ) ;
#7983 = PLANE ( 'NONE',  #16662 ) ;
#7984 = DIRECTION ( 'NONE',  ( -0.000000000000000000, -0.000000000000000000, 1.000000000000000000 ) ) ;
#7985 = LINE ( 'NONE', #19223, #11976 ) ;
#7986 = ORIENTED_EDGE ( 'NONE', *, *, #12317, .T. ) ;
#7987 = CARTESIAN_POINT ( 'NONE',  ( 9.999999999999998224, 67.51707036274449081, -25.00890260772307627 ) ) ;
#7988 = AXIS2_PLACEMENT_3D ( 'NONE', #7767, #18910, #12862 ) ;
#7989 = CARTESIAN_POINT ( 'NONE',  ( -6.358192988180021210, -4.248408729364580694, 1.042606250180315497 ) ) ;
#7990 = ORIENTED_EDGE ( 'NONE', *, *, #5589, .T. ) ;
#7991 = LINE ( 'NONE', #2800, #3838 ) ;
#7992 = DIRECTION ( 'NONE',  ( 0.000000000000000000, 0.000000000000000000, 1.000000000000000000 ) ) ;
#7993 = VECTOR ( 'NONE', #4318, 1000.000000000000000 ) ;
#7994 = ORIENTED_EDGE ( 'NONE', *, *, #1991, .T. ) ;
#7995 = EDGE_CURVE ( 'NONE', #9883, #4283, #5764, .T. ) ;
#7996 = CARTESIAN_POINT ( 'NONE',  ( 19.99999999999999645, 63.17103598352149874, -16.33561182745074447 ) ) ;
#7997 = CARTESIAN_POINT ( 'NONE',  ( 10.00000000000000178, -164.9999999999999716, 73.20000000000000284 ) ) ;
#7998 = CARTESIAN_POINT ( 'NONE',  ( 19.99999999999999645, 0.000000000000000000, 0.000000000000000000 ) ) ;
#7999 = EDGE_LOOP ( 'NONE', ( #16814, #1033 ) ) ;
#8000 = CARTESIAN_POINT ( 'NONE',  ( 0.000000000000000000, 0.000000000000000000, -68.00000000000000000 ) ) ;
#8001 = ORIENTED_EDGE ( 'NONE', *, *, #10493, .F. ) ;
#8002 = DIRECTION ( 'NONE',  ( -0.000000000000000000, 0.000000000000000000, -1.000000000000000000 ) ) ;
#8003 = VERTEX_POINT ( 'NONE', #15315 ) ;
#8004 = CIRCLE ( 'NONE', #19833, 72.00000000007199219 ) ;
#8005 = CARTESIAN_POINT ( 'NONE',  ( -7.459310946700270506E-14, -4.618802153517020948, -5.242734410091827613 ) ) ;
#8006 = AXIS2_PLACEMENT_3D ( 'NONE', #4628, #4731, #20937 ) ;
#8007 = CIRCLE ( 'NONE', #10724, 27.60000000002760601 ) ;
#8008 = CARTESIAN_POINT ( 'NONE',  ( 19.99999999999999645, 51.81019761368321497, 38.98425606966075918 ) ) ;
#8009 = CARTESIAN_POINT ( 'NONE',  ( -13.67243654778936168, -5.663308646854336992, -17.83627058115845898 ) ) ;
#8010 = ORIENTED_EDGE ( 'NONE', *, *, #8959, .F. ) ;
#8011 = CARTESIAN_POINT ( 'NONE',  ( -5.303300859536632217, -5.303300858261584594, -14.94182499981969592 ) ) ;
#8012 = AXIS2_PLACEMENT_3D ( 'NONE', #17840, #3311, #9773 ) ;
#8013 = DIRECTION ( 'NONE',  ( 0.000000000000000000, 0.000000000000000000, 1.000000000000000000 ) ) ;
#8014 = VERTEX_POINT ( 'NONE', #18714 ) ;
#8015 = CARTESIAN_POINT ( 'NONE',  ( 0.000000000000000000, 0.000000000000000000, 0.000000000000000000 ) ) ;
#8016 = AXIS2_PLACEMENT_3D ( 'NONE', #12012, #15192, #5334 ) ;
#8017 = EDGE_CURVE ( 'NONE', #7766, #9694, #20400, .T. ) ;
#8018 = VECTOR ( 'NONE', #4096, 1000.000000000000000 ) ;
#8019 = DIRECTION ( 'NONE',  ( 0.000000000000000000, -1.000000000000000000, 0.000000000000000000 ) ) ;
#8020 = CARTESIAN_POINT ( 'NONE',  ( 0.000000000000000000, 0.000000000000000000, -68.00000000000000000 ) ) ;
#8021 = DIRECTION ( 'NONE',  ( -1.000000000000000000, -3.552713678800500929E-15, 0.000000000000000000 ) ) ;
#8022 = CIRCLE ( 'NONE', #2270, 2.649999999999999467 ) ;
#8023 = ORIENTED_EDGE ( 'NONE', *, *, #6244, .T. ) ;
#8024 = CARTESIAN_POINT ( 'NONE',  ( 9.999999999999998224, -29.55812890832026341, 65.65300461859676773 ) ) ;
#8025 = LINE ( 'NONE', #11797, #16171 ) ;
#8026 = ORIENTED_EDGE ( 'NONE', *, *, #12068, .T. ) ;
#8027 = EDGE_CURVE ( 'NONE', #8014, #5950, #18346, .T. ) ;
#8028 = FACE_OUTER_BOUND ( 'NONE', #8804, .T. ) ;
#8029 = DIRECTION ( 'NONE',  ( 0.000000000000000000, 0.2697967711570182225, 0.9629172873478010208 ) ) ;
#8030 = DIRECTION ( 'NONE',  ( -1.000000000000000000, -0.000000000000000000, -0.000000000000000000 ) ) ;
#8031 = AXIS2_PLACEMENT_3D ( 'NONE', #539, #6986, #13474 ) ;
#8032 = ORIENTED_EDGE ( 'NONE', *, *, #5592, .T. ) ;
#8033 = CARTESIAN_POINT ( 'NONE',  ( 0.000000000000000000, 0.000000000000000000, 81.99999999999998579 ) ) ;
#8034 =( NAMED_UNIT ( * ) PLANE_ANGLE_UNIT ( ) SI_UNIT ( $, .RADIAN. ) );
#8035 = CARTESIAN_POINT ( 'NONE',  ( 0.000000000000000000, 0.000000000000000000, 0.000000000000000000 ) ) ;
#8036 = DIRECTION ( 'NONE',  ( 1.000000000000000000, 0.000000000000000000, 0.000000000000000000 ) ) ;
#8037 = CARTESIAN_POINT ( 'NONE',  ( 18.00000000043041481, 3.580422610670020322, -14.68598124981969377 ) ) ;
#8038 = ADVANCED_FACE ( 'NONE', ( #10863 ), #10972, .F. ) ;
#8040 = ORIENTED_EDGE ( 'NONE', *, *, #12601, .F. ) ;
#8039 = CIRCLE ( 'NONE', #4666, 27.60000000002759535 ) ;
#8041 = AXIS2_PLACEMENT_3D ( 'NONE', #8892, #16628, #15153 ) ;
#8042 = CARTESIAN_POINT ( 'NONE',  ( 9.999999999999998224, 27.80658314415319055, -66.41380830714092554 ) ) ;
#8043 = LINE ( 'NONE', #18965, #7004 ) ;
#8044 = CARTESIAN_POINT ( 'NONE',  ( 2.943691928843430450, 14.79893867722910095, -1.364510668480926281 ) ) ;
#8045 = DIRECTION ( 'NONE',  ( 1.000000000000000000, 0.000000000000000000, 0.000000000000000000 ) ) ;
#8046 = CIRCLE ( 'NONE', #18194, 2.099999999999990763 ) ;
#8047 = ORIENTED_EDGE ( 'NONE', *, *, #1345, .T. ) ;
#8048 = DIRECTION ( 'NONE',  ( 0.000000000000000000, -0.9790840876823205807, -0.2034560130526446575 ) ) ;
#8049 = AXIS2_PLACEMENT_3D ( 'NONE', #19547, #5028, #16363 ) ;
#8050 = CARTESIAN_POINT ( 'NONE',  ( -1.491842754445842800, 7.500000000179346316, 22.83791875018031448 ) ) ;
#8051 = CYLINDRICAL_SURFACE ( 'NONE', #9046, 27.60000000002760245 ) ;
#8052 = ORIENTED_EDGE ( 'NONE', *, *, #15416, .F. ) ;
#8053 = EDGE_CURVE ( 'NONE', #9946, #645, #58, .T. ) ;
#8054 = CARTESIAN_POINT ( 'NONE',  ( 0.000000000000000000, 0.000000000000000000, 90.00000000000000000 ) ) ;
#8055 = AXIS2_PLACEMENT_3D ( 'NONE', #17271, #960, #4002 ) ;
#8056 = ORIENTED_EDGE ( 'NONE', *, *, #19310, .T. ) ;
#8057 = FACE_OUTER_BOUND ( 'NONE', #7680, .T. ) ;
#8058 = DIRECTION ( 'NONE',  ( 0.000000000000000000, 0.000000000000000000, 1.000000000000000000 ) ) ;
#8059 = ADVANCED_FACE ( 'NONE', ( #17650 ), #20924, .T. ) ;
#8060 = VERTEX_POINT ( 'NONE', #7689 ) ;
#8061 = ORIENTED_EDGE ( 'NONE', *, *, #585, .T. ) ;
#8062 = CARTESIAN_POINT ( 'NONE',  ( 0.000000000000000000, 0.000000000000000000, 0.000000000000000000 ) ) ;
#8063 = ADVANCED_FACE ( 'NONE', ( #17336 ), #4611, .T. ) ;
#8064 = APPLICATION_CONTEXT ( 'automotive_design' ) ;
#8065 = EDGE_CURVE ( 'NONE', #17850, #9196, #11178, .T. ) ;
#8066 = DIRECTION ( 'NONE',  ( 1.000000000000000000, 0.000000000000000000, 0.000000000000000000 ) ) ;
#8067 = DIRECTION ( 'NONE',  ( 1.000000000000000000, 0.000000000000000000, 0.000000000000000000 ) ) ;
#8068 = CARTESIAN_POINT ( 'NONE',  ( 10.32494394706616347, -4.276731815070950127, -20.61832774935258072 ) ) ;
#8069 = CARTESIAN_POINT ( 'NONE',  ( 7.902369978624323110, 7.902369976724394895, 8.191765249713197861 ) ) ;
#8070 = LINE ( 'NONE', #3191, #1752 ) ;
#8071 = EDGE_CURVE ( 'NONE', #5402, #16359, #4815, .T. ) ;
#8072 = DIRECTION ( 'NONE',  ( -1.000000000000000000, 0.000000000000000000, 0.000000000000000000 ) ) ;
#8073 = DIRECTION ( 'NONE',  ( 0.000000000000000000, 0.000000000000000000, 1.000000000000000000 ) ) ;
#8074 = EDGE_CURVE ( 'NONE', #4217, #18949, #3437, .T. ) ;
#8075 = ORIENTED_EDGE ( 'NONE', *, *, #20744, .F. ) ;
#8076 = CYLINDRICAL_SURFACE ( 'NONE', #20008, 7.500000000000000000 ) ;
#8077 = VERTEX_POINT ( 'NONE', #14375 ) ;
#8078 = CARTESIAN_POINT ( 'NONE',  ( -16.62983158437510056, 6.888301784570729502, 19.18511250018031333 ) ) ;
#8079 = DIRECTION ( 'NONE',  ( -0.000000000000000000, -0.000000000000000000, 1.000000000000000000 ) ) ;
#8080 = VERTEX_POINT ( 'NONE', #6194 ) ;
#8081 = DIRECTION ( 'NONE',  ( 1.000000000000000000, 0.000000000000000000, 0.000000000000000000 ) ) ;
#8082 = ORIENTED_EDGE ( 'NONE', *, *, #6989, .T. ) ;
#8083 = DIRECTION ( 'NONE',  ( -1.000000000000000000, 0.000000000000000000, 0.000000000000000000 ) ) ;
#8084 = CARTESIAN_POINT ( 'NONE',  ( 41.14327188351807507, -13.96402716752546169, 80.34089272068401044 ) ) ;
#8085 = EDGE_CURVE ( 'NONE', #14352, #4723, #20703, .T. ) ;
#8086 = EDGE_LOOP ( 'NONE', ( #12766, #11412 ) ) ;
#8087 = EDGE_LOOP ( 'NONE', ( #5094, #1931, #16672, #5364 ) ) ;
#8088 = CYLINDRICAL_SURFACE ( 'NONE', #556, 7.500000000000000000 ) ;
#8089 = ADVANCED_FACE ( 'NONE', ( #20819 ), #6300, .T. ) ;
#8090 = FACE_OUTER_BOUND ( 'NONE', #20009, .T. ) ;
#8091 = FACE_OUTER_BOUND ( 'NONE', #17998, .T. ) ;
#8092 = VERTEX_POINT ( 'NONE', #20508 ) ;
#8093 = CARTESIAN_POINT ( 'NONE',  ( -1.491842754445841246, 7.500000000179339210, 16.57301875018031012 ) ) ;
#8094 = DIRECTION ( 'NONE',  ( 0.000000000000000000, 0.000000000000000000, -1.000000000000000000 ) ) ;
#8095 = DIRECTION ( 'NONE',  ( 0.000000000000000000, 0.000000000000000000, -1.000000000000000000 ) ) ;
#8096 = DIRECTION ( 'NONE',  ( 0.000000000000000000, 0.7812527682501551052, 0.6242147964454778375 ) ) ;
#8097 = EDGE_CURVE ( 'NONE', #11587, #20459, #14292, .T. ) ;
#8098 = ORIENTED_EDGE ( 'NONE', *, *, #5847, .F. ) ;
#8099 = DIRECTION ( 'NONE',  ( 0.000000000000000000, -0.3984010898462296835, -0.9172113015054581542 ) ) ;
#8100 = CARTESIAN_POINT ( 'NONE',  ( -12.72792205982779912, 12.72792206288790950, 17.86957500018031553 ) ) ;
#8101 = DIRECTION ( 'NONE',  ( 0.000000000000000000, 0.8878852184023731109, 0.4600650377311562012 ) ) ;
#8102 = ORIENTED_EDGE ( 'NONE', *, *, #6381, .F. ) ;
#8103 = CARTESIAN_POINT ( 'NONE',  ( -30.00000000000000000, 36.35083268962917202, 90.00000000000000000 ) ) ;
#8104 = ORIENTED_EDGE ( 'NONE', *, *, #4453, .F. ) ;
#8105 = DIRECTION ( 'NONE',  ( 0.000000000000000000, 1.000000000000000000, 0.000000000000000000 ) ) ;
#8106 = ORIENTED_EDGE ( 'NONE', *, *, #13101, .T. ) ;
#8107 = LINE ( 'NONE', #13090, #11437 ) ;
#8108 = EDGE_CURVE ( 'NONE', #19446, #16924, #20708, .T. ) ;
#8109 = CARTESIAN_POINT ( 'NONE',  ( -7.500000000000007994, -4.022542210876018231E-17, 20.77620000000231570 ) ) ;
#8110 = CARTESIAN_POINT ( 'NONE',  ( -8.382925368423274293, 12.54593441764187745, -15.77455183115845649 ) ) ;
#8111 = ORIENTED_EDGE ( 'NONE', *, *, #11938, .F. ) ;
#8112 = CARTESIAN_POINT ( 'NONE',  ( -6.359999999999997655, 4.663913298532544267E-15, 0.000000000000000000 ) ) ;
#8113 = CARTESIAN_POINT ( 'NONE',  ( 3.599999999999902389, -10.82531754730554496, 43.00000000000000000 ) ) ;
#8114 = ORIENTED_EDGE ( 'NONE', *, *, #11936, .T. ) ;
#8115 = DIRECTION ( 'NONE',  ( 0.000000000000000000, 0.000000000000000000, 1.000000000000000000 ) ) ;
#8116 = CARTESIAN_POINT ( 'NONE',  ( -16.62983158603122291, -6.888301780572501087, 18.00698750018031546 ) ) ;
#8117 = DIRECTION ( 'NONE',  ( -1.000000000000000000, 0.000000000000000000, 0.000000000000000000 ) ) ;
#8118 = CIRCLE ( 'NONE', #326, 27.60000000002759180 ) ;
#8119 = ORIENTED_EDGE ( 'NONE', *, *, #12338, .T. ) ;
#8120 = CARTESIAN_POINT ( 'NONE',  ( 30.00000000000000000, -105.0000000000000000, -90.00000000000001421 ) ) ;
#8121 = VERTEX_POINT ( 'NONE', #19028 ) ;
#8122 = DIRECTION ( 'NONE',  ( 0.000000000000000000, -0.8169698930104469792, 0.5766803221148600889 ) ) ;
#8123 = FACE_OUTER_BOUND ( 'NONE', #6780, .T. ) ;
#8124 = DIRECTION ( 'NONE',  ( -1.000000000000000000, 0.000000000000000000, 0.000000000000000000 ) ) ;
#8125 = ORIENTED_EDGE ( 'NONE', *, *, #11555, .T. ) ;
#8126 = DIRECTION ( 'NONE',  ( 1.000000000000000000, 0.000000000000000000, 0.000000000000000000 ) ) ;
#8127 = EDGE_CURVE ( 'NONE', #1793, #19110, #19140, .T. ) ;
#8128 = LINE ( 'NONE', #14601, #3451 ) ;
#8129 = SHAPE_DEFINITION_REPRESENTATION ( #9997, #2344 ) ;
#8130 = CARTESIAN_POINT ( 'NONE',  ( 17.99999999956958519, -3.580422614997676778, -14.09691874981969129 ) ) ;
#8131 = ORIENTED_EDGE ( 'NONE', *, *, #2354, .F. ) ;
#8132 = AXIS2_PLACEMENT_3D ( 'NONE', #10851, #15836, #1331 ) ;
#8133 = DIRECTION ( 'NONE',  ( 0.000000000000000000, 0.000000000000000000, 1.000000000000000000 ) ) ;
#8134 = CARTESIAN_POINT ( 'NONE',  ( 50.00000000000000000, 31.35083268962909742, -2.067608244099269852E-13 ) ) ;
#8135 = CARTESIAN_POINT ( 'NONE',  ( 5.663308650141530620, 13.67243654642775041, -1.069979418480925926 ) ) ;
#8136 = CARTESIAN_POINT ( 'NONE',  ( -10.00000000000000000, 0.000000000000000000, 0.000000000000000000 ) ) ;
#8137 = PRESENTATION_LAYER_ASSIGNMENT (  '', '', ( #15229 ) ) ;
#8138 = EDGE_LOOP ( 'NONE', ( #8537, #14214, #15435, #14509 ) ) ;
#8139 = FACE_OUTER_BOUND ( 'NONE', #18382, .T. ) ;
#8140 = CARTESIAN_POINT ( 'NONE',  ( -11.49999999999998934, -85.00000000000000000, 5.000000000000000000 ) ) ;
#8141 = CARTESIAN_POINT ( 'NONE',  ( 38.67130833460402073, -17.89826649859318408, 72.22104433765980502 ) ) ;
#8142 = ORIENTED_EDGE ( 'NONE', *, *, #19706, .F. ) ;
#8143 = CARTESIAN_POINT ( 'NONE',  ( 19.99999999999999645, -55.05624179291956466, -35.01774179823839717 ) ) ;
#8144 = ORIENTED_EDGE ( 'NONE', *, *, #3117, .F. ) ;
#8145 = CARTESIAN_POINT ( 'NONE',  ( 6.232799999999996565, 1.325911618322048272E-15, -10.79377999999999993 ) ) ;
#8146 = DIRECTION ( 'NONE',  ( 0.000000000000000000, 0.000000000000000000, 1.000000000000000000 ) ) ;
#8147 = CIRCLE ( 'NONE', #19312, 2.055000000000000160 ) ;
#8148 = ORIENTED_EDGE ( 'NONE', *, *, #4230, .F. ) ;
#8149 = ORIENTED_EDGE ( 'NONE', *, *, #1632, .F. ) ;
#8150 = LINE ( 'NONE', #6556, #577 ) ;
#8151 = CARTESIAN_POINT ( 'NONE',  ( 6.165579999999996730, 0.000000000000000000, 7.500000000000000888 ) ) ;
#8152 = CIRCLE ( 'NONE', #8807, 11.49999999999999645 ) ;
#8153 = SURFACE_SIDE_STYLE ('',( #14937 ) ) ;
#8154 = DIRECTION ( 'NONE',  ( -1.000000000000000000, 0.000000000000000000, 0.000000000000000000 ) ) ;
#8155 = CARTESIAN_POINT ( 'NONE',  ( -10.00000000000000000, 0.000000000000000000, 0.000000000000000000 ) ) ;
#8156 = CARTESIAN_POINT ( 'NONE',  ( 11.17563879731705789, -1.343450868547281933E-09, -21.20739024935257788 ) ) ;
#8157 = EDGE_CURVE ( 'NONE', #14635, #9288, #4505, .T. ) ;
#8158 = CARTESIAN_POINT ( 'NONE',  ( -4.276731812588563386, 10.32494394809438987, -3.000422250286804093 ) ) ;
#8159 = ADVANCED_FACE ( 'NONE', ( #1130 ), #9388, .T. ) ;
#8160 = SHAPE_REPRESENTATION ( 'tail shaft', ( #12461 ), #3268 ) ;
#8161 = DIRECTION ( 'NONE',  ( -1.000000000000000000, 0.000000000000000000, -0.000000000000000000 ) ) ;
#8162 = DIRECTION ( 'NONE',  ( 0.000000000000000000, 0.000000000000000000, -1.000000000000000000 ) ) ;
#8163 = AXIS2_PLACEMENT_3D ( 'NONE', #14475, #249, #9787 ) ;
#8164 = ORIENTED_EDGE ( 'NONE', *, *, #20339, .T. ) ;
#8165 = DIRECTION ( 'NONE',  ( 1.000000000000000000, 0.000000000000000000, 0.000000000000000000 ) ) ;
#8166 = CARTESIAN_POINT ( 'NONE',  ( 16.62983158437509346, -6.888301784570739272, -25.13198749981969016 ) ) ;
#8167 = CYLINDRICAL_SURFACE ( 'NONE', #11991, 27.60000000002759890 ) ;
#8168 = AXIS2_PLACEMENT_3D ( 'NONE', #17071, #15259, #6993 ) ;
#8169 = ADVANCED_FACE ( 'NONE', ( #7787 ), #14060, .T. ) ;
#8170 = ORIENTED_EDGE ( 'NONE', *, *, #1077, .F. ) ;
#8171 = CARTESIAN_POINT ( 'NONE',  ( -4.000000000000000000, 2.309401076758496263, -0.3572655899081631503 ) ) ;
#8172 = ORIENTED_EDGE ( 'NONE', *, *, #3481, .F. ) ;
#8173 = LINE ( 'NONE', #13792, #723 ) ;
#8174 = CARTESIAN_POINT ( 'NONE',  ( 30.62662295113251787, -40.93503228410152417, -66.38288848018791555 ) ) ;
#8175 = ORIENTED_EDGE ( 'NONE', *, *, #17652, .T. ) ;
#8176 = VECTOR ( 'NONE', #9101, 1000.000000000000000 ) ;
#8177 = ORIENTED_EDGE ( 'NONE', *, *, #127, .F. ) ;
#8178 = CARTESIAN_POINT ( 'NONE',  ( 0.000000000000000000, 0.000000000000000000, -5.574599999999999334 ) ) ;
#8179 = CARTESIAN_POINT ( 'NONE',  ( 49.19234958605026264, -1.326995226329880762, -84.99999999999998579 ) ) ;
#8180 = CIRCLE ( 'NONE', #9197, 72.00000000007199219 ) ;
#8181 = EDGE_CURVE ( 'NONE', #19870, #16541, #14964, .T. ) ;
#8182 = CARTESIAN_POINT ( 'NONE',  ( -7.500000000000007105, -3.289131931996631318E-15, 11.35120000000231677 ) ) ;
#8183 = AXIS2_PLACEMENT_3D ( 'NONE', #15545, #7487, #14191 ) ;
#8184 = ORIENTED_EDGE ( 'NONE', *, *, #11919, .T. ) ;
#8185 = EDGE_CURVE ( 'NONE', #1607, #12002, #1774, .T. ) ;
#8186 = CARTESIAN_POINT ( 'NONE',  ( 19.99999999999999645, 42.42902769288603082, -49.02903636734153281 ) ) ;
#8187 = ADVANCED_FACE ( 'NONE', ( #18117 ), #19308, .F. ) ;
#8188 = DIRECTION ( 'NONE',  ( -0.000000000000000000, -0.000000000000000000, -1.000000000000000000 ) ) ;
#8189 = CIRCLE ( 'NONE', #15632, 65.24900000006525147 ) ;
#8190 = CARTESIAN_POINT ( 'NONE',  ( 9.999999999999998224, 70.29359119158506530, -15.58239511117214704 ) ) ;
#8191 = LINE ( 'NONE', #2453, #2509 ) ;
#8192 = ORIENTED_EDGE ( 'NONE', *, *, #10651, .F. ) ;
#8193 = DIRECTION ( 'NONE',  ( 1.000000000000000000, 0.000000000000000000, 0.000000000000000000 ) ) ;
#8194 = EDGE_CURVE ( 'NONE', #5437, #8657, #310, .T. ) ;
#8195 = DIRECTION ( 'NONE',  ( 0.000000000000000000, 0.000000000000000000, 1.000000000000000000 ) ) ;
#8196 = CARTESIAN_POINT ( 'NONE',  ( 19.99999999999999645, -1.971042061628798470, 64.80882494896106039 ) ) ;
#8197 = ORIENTED_EDGE ( 'NONE', *, *, #7419, .F. ) ;
#8198 = DIRECTION ( 'NONE',  ( 0.000000000000000000, 0.000000000000000000, 1.000000000000000000 ) ) ;
#8199 = ORIENTED_EDGE ( 'NONE', *, *, #19482, .T. ) ;
#8200 = DIRECTION ( 'NONE',  ( -1.000000000000000000, 0.000000000000000000, 0.000000000000000000 ) ) ;
#8201 = VERTEX_POINT ( 'NONE', #3686 ) ;
#8202 = DIRECTION ( 'NONE',  ( 0.000000000000000000, 0.000000000000000000, 1.000000000000000000 ) ) ;
#8203 = ADVANCED_FACE ( 'NONE', ( #1533 ), #7983, .F. ) ;
#8204 = LINE ( 'NONE', #11805, #14342 ) ;
#8205 = CARTESIAN_POINT ( 'NONE',  ( 8.382925368423272516, -12.54593441764187745, -11.06205183115845614 ) ) ;
#8206 = VECTOR ( 'NONE', #15429, 1000.000000000000000 ) ;
#8208 = VERTEX_POINT ( 'NONE', #8457 ) ;
#8207 = AXIS2_PLACEMENT_3D ( 'NONE', #12679, #17231, #15739 ) ;
#8209 = CYLINDRICAL_SURFACE ( 'NONE', #1861, 21.50000000000000000 ) ;
#8210 = EDGE_CURVE ( 'NONE', #14524, #7039, #16145, .T. ) ;
#8211 = CARTESIAN_POINT ( 'NONE',  ( 45.22159793441011999, -8.673994507468391291, -78.07221698934968401 ) ) ;
#8212 = AXIS2_PLACEMENT_3D ( 'NONE', #3447, #8525, #8327 ) ;
#8213 = ORIENTED_EDGE ( 'NONE', *, *, #6344, .F. ) ;
#8214 = CARTESIAN_POINT ( 'NONE',  ( 19.99999999999999645, 49.77519642624064744, -42.18840861821734478 ) ) ;
#8215 = CARTESIAN_POINT ( 'NONE',  ( 18.00000000000000000, -2.163824016901520184E-09, 23.30855000018031475 ) ) ;
#8216 = FACE_OUTER_BOUND ( 'NONE', #18658, .T. ) ;
#8217 = CYLINDRICAL_SURFACE ( 'NONE', #3929, 10.00000000000000178 ) ;
#8218 = CIRCLE ( 'NONE', #10643, 27.60000000002759890 ) ;
#8219 = VERTEX_POINT ( 'NONE', #6763 ) ;
#8220 = LINE ( 'NONE', #8120, #1277 ) ;
#8221 = EDGE_LOOP ( 'NONE', ( #12856, #18052 ) ) ;
#8222 = VECTOR ( 'NONE', #17765, 1000.000000000000000 ) ;
#8223 = DIRECTION ( 'NONE',  ( 0.000000000000000000, 1.000000000000000000, 1.040834085586084454E-15 ) ) ;
#8224 = AXIS2_PLACEMENT_3D ( 'NONE', #14058, #255, #11280 ) ;
#8225 = CARTESIAN_POINT ( 'NONE',  ( 19.99999999999999645, 59.36728637278074672, -40.73727173906726051 ) ) ;
#8226 = DIRECTION ( 'NONE',  ( -1.000000000000000000, 0.000000000000000000, 0.000000000000000000 ) ) ;
#8227 = VERTEX_POINT ( 'NONE', #5482 ) ;
#8228 = DIRECTION ( 'NONE',  ( 1.000000000000000000, 0.000000000000000000, 0.000000000000000000 ) ) ;
#8229 = PLANE ( 'NONE',  #11269 ) ;
#8230 = APPLICATION_PROTOCOL_DEFINITION ( 'draft international standard', 'automotive_design', 1998, #10067 ) ;
#8231 = AXIS2_PLACEMENT_3D ( 'NONE', #6042, #20564, #17498 ) ;
#8232 = CARTESIAN_POINT ( 'NONE',  ( -6.888301784570739272, -16.62983158437509701, -11.44613749981969519 ) ) ;
#8233 = AXIS2_PLACEMENT_3D ( 'NONE', #11235, #3291, #13149 ) ;
#8234 = ORIENTED_EDGE ( 'NONE', *, *, #8181, .F. ) ;
#8235 = DIRECTION ( 'NONE',  ( 1.000000000000000000, 0.000000000000000000, 0.000000000000000000 ) ) ;
#8236 = AXIS2_PLACEMENT_3D ( 'NONE', #13691, #16651, #8909 ) ;
#8237 = VECTOR ( 'NONE', #3701, 1000.000000000000000 ) ;
#8238 = CARTESIAN_POINT ( 'NONE',  ( -10.46442989454075168, -10.46442989202483709, -5.193416918480926903 ) ) ;
#8239 = CARTESIAN_POINT ( 'NONE',  ( 3.599999999999909051, -10.82531754730554496, 46.00000000000000711 ) ) ;
#8240 = ADVANCED_FACE ( 'NONE', ( #16616, #19694 ), #1901, .T. ) ;
#8241 = EDGE_LOOP ( 'NONE', ( #9081, #13985, #11177, #11832 ) ) ;
#8242 = EDGE_CURVE ( 'NONE', #15031, #4041, #14838, .T. ) ;
#8243 = DIRECTION ( 'NONE',  ( -1.000000000000000000, 0.000000000000000000, 0.000000000000000000 ) ) ;
#8244 = CARTESIAN_POINT ( 'NONE',  ( 0.000000000000000000, 0.000000000000000000, -68.00000000000000000 ) ) ;
#8245 = CARTESIAN_POINT ( 'NONE',  ( 32.99404949636548423, -30.67485788781106848, 67.67723498345976907 ) ) ;
#8246 = EDGE_LOOP ( 'NONE', ( #16793, #16831, #717, #20150 ) ) ;
#8247 = CIRCLE ( 'NONE', #17046, 27.60000000002759890 ) ;
#8248 = DIRECTION ( 'NONE',  ( 0.000000000000000000, 1.000000000000000000, 0.000000000000000000 ) ) ;
#8249 = VERTEX_POINT ( 'NONE', #5382 ) ;
#8250 = DIRECTION ( 'NONE',  ( -1.000000000000000000, 0.000000000000000000, 0.000000000000000000 ) ) ;
#8251 = CARTESIAN_POINT ( 'NONE',  ( 24.99999999999999645, -99.99999999999998579, -49.89999999999999858 ) ) ;
#8252 = ORIENTED_EDGE ( 'NONE', *, *, #17325, .F. ) ;
#8253 = EDGE_LOOP ( 'NONE', ( #590, #15134, #11903, #11400 ) ) ;
#8254 = CYLINDRICAL_SURFACE ( 'NONE', #5991, 27.60000000002759535 ) ;
#8255 = AXIS2_PLACEMENT_3D ( 'NONE', #6788, #13273, #16547 ) ;
#8256 = AXIS2_PLACEMENT_3D ( 'NONE', #13184, #9888, #8401 ) ;
#8257 = DIRECTION ( 'NONE',  ( 0.000000000000000000, 0.8169698930104392076, 0.5766803221148710801 ) ) ;
#8258 = SURFACE_SIDE_STYLE ('',( #16415 ) ) ;
#8259 = CARTESIAN_POINT ( 'NONE',  ( 0.000000000000000000, -14.55863677812078016, -63.60407295269120453 ) ) ;
#8260 = CYLINDRICAL_SURFACE ( 'NONE', #12236, 2.649999999999999467 ) ;
#8261 = CARTESIAN_POINT ( 'NONE',  ( -6.929096494179684207, -2.870125741905212635, 20.18713750018031305 ) ) ;
#8262 = AXIS2_PLACEMENT_3D ( 'NONE', #2690, #128, #14652 ) ;
#8263 = ADVANCED_FACE ( 'NONE', ( #20906 ), #13242, .F. ) ;
#8264 = CARTESIAN_POINT ( 'NONE',  ( -10.32494394809439164, -4.276731812588563386, -5.356672250286801606 ) ) ;
#8265 = DIRECTION ( 'NONE',  ( 0.000000000000000000, 0.000000000000000000, 1.000000000000000000 ) ) ;
#8266 = FACE_OUTER_BOUND ( 'NONE', #17954, .T. ) ;
#8267 = CIRCLE ( 'NONE', #10301, 7.500000000000000000 ) ;
#8268 = ORIENTED_EDGE ( 'NONE', *, *, #4439, .F. ) ;
#8269 = DIRECTION ( 'NONE',  ( 0.000000000000000000, 0.000000000000000000, 1.000000000000000000 ) ) ;
#8270 = CARTESIAN_POINT ( 'NONE',  ( 6.888301784570728614, 16.62983158437510056, 12.11636250018031369 ) ) ;
#8271 = CARTESIAN_POINT ( 'NONE',  ( 30.00000000000000000, -39.99999999999999289, 54.09999999999999432 ) ) ;
#8272 = ORIENTED_EDGE ( 'NONE', *, *, #678, .T. ) ;
#8273 = CARTESIAN_POINT ( 'NONE',  ( 45.22159793441011999, -8.673994507468384185, 84.62946326583127643 ) ) ;
#8274 = VERTEX_POINT ( 'NONE', #13553 ) ;
#8275 = CARTESIAN_POINT ( 'NONE',  ( 21.00000000000000355, 0.000000000000000000, 0.000000000000000000 ) ) ;
#8276 = DIRECTION ( 'NONE',  ( -1.000000000000000000, -0.000000000000000000, 0.000000000000000000 ) ) ;
#8277 = ORIENTED_EDGE ( 'NONE', *, *, #4688, .F. ) ;
#8278 = ORIENTED_EDGE ( 'NONE', *, *, #14144, .F. ) ;
#8279 = DIRECTION ( 'NONE',  ( -1.000000000000000000, 0.000000000000000000, 0.000000000000000000 ) ) ;
#8280 = EDGE_CURVE ( 'NONE', #6577, #3526, #10063, .T. ) ;
#8281 = CARTESIAN_POINT ( 'NONE',  ( 50.00000000000000000, 31.35083268962909742, -2.067608244099269852E-13 ) ) ;
#8282 = AXIS2_PLACEMENT_3D ( 'NONE', #16068, #17053, #18638 ) ;
#8283 = LINE ( 'NONE', #6386, #11624 ) ;
#8284 = ADVANCED_FACE ( 'NONE', ( #8669 ), #11756, .T. ) ;
#8285 = EDGE_CURVE ( 'NONE', #1316, #7136, #20025, .T. ) ;
#8286 = ORIENTED_EDGE ( 'NONE', *, *, #6822, .T. ) ;
#8287 = CARTESIAN_POINT ( 'NONE',  ( -4.248408730893245000, -6.358192987158590270, 3.613643750180311809 ) ) ;
#8288 = FACE_OUTER_BOUND ( 'NONE', #4839, .T. ) ;
#8289 = CARTESIAN_POINT ( 'NONE',  ( -10.00000000000000000, 0.000000000000000000, 0.000000000000000000 ) ) ;
#8290 = FACE_OUTER_BOUND ( 'NONE', #7352, .T. ) ;
#8291 = CARTESIAN_POINT ( 'NONE',  ( 6.249999999999902300, -10.82531754730554496, 46.00000000000000711 ) ) ;
#8292 = CARTESIAN_POINT ( 'NONE',  ( 19.99999999999999645, 49.77519642624064744, -42.18840861821734478 ) ) ;
#8293 = ORIENTED_EDGE ( 'NONE', *, *, #3492, .T. ) ;
#8294 = CARTESIAN_POINT ( 'NONE',  ( 5.200000000000002842, 0.000000000000000000, 0.000000000000000000 ) ) ;
#8295 = ORIENTED_EDGE ( 'NONE', *, *, #17680, .T. ) ;
#8296 = CYLINDRICAL_SURFACE ( 'NONE', #11067, 2.649999999999994582 ) ;
#8297 = CARTESIAN_POINT ( 'NONE',  ( 19.99999999999999645, -65.23577793412346182, 1.313498510941474740 ) ) ;
#8298 = EDGE_LOOP ( 'NONE', ( #8552, #8949, #13841, #13503 ) ) ;
#8299 = DIRECTION ( 'NONE',  ( -0.000000000000000000, -0.000000000000000000, -1.000000000000000000 ) ) ;
#8300 = ORIENTED_EDGE ( 'NONE', *, *, #4818, .T. ) ;
#8301 = VECTOR ( 'NONE', #4379, 1000.000000000000000 ) ;
#8302 = DIRECTION ( 'NONE',  ( -0.000000000000000000, -0.000000000000000000, -1.000000000000000000 ) ) ;
#8303 = EDGE_LOOP ( 'NONE', ( #804, #9597 ) ) ;
#8304 = ADVANCED_FACE ( 'NONE', ( #9565 ), #524, .T. ) ;
#8305 = EDGE_CURVE ( 'NONE', #11056, #19208, #19037, .T. ) ;
#8306 = CARTESIAN_POINT ( 'NONE',  ( 37.16069494243885885, -120.3585804411932116, 78.81711354060604435 ) ) ;
#8307 = CIRCLE ( 'NONE', #13735, 27.60000000002759890 ) ;
#8308 = ADVANCED_FACE ( 'NONE', ( #19906 ), #20437, .T. ) ;
#8309 = LINE ( 'NONE', #18070, #6538 ) ;
#8310 = CARTESIAN_POINT ( 'NONE',  ( 2.222972768810839383, -11.17563879758428769, 9.129328500647432065 ) ) ;
#8311 = ORIENTED_EDGE ( 'NONE', *, *, #15439, .F. ) ;
#8312 = AXIS2_PLACEMENT_3D ( 'NONE', #16422, #19503, #6264 ) ;
#8313 = CARTESIAN_POINT ( 'NONE',  ( 0.000000000000000000, 56.63599015375672963, 31.56633360682482703 ) ) ;
#8314 = CARTESIAN_POINT ( 'NONE',  ( 0.000000000000000000, 0.000000000000000000, 0.000000000000000000 ) ) ;
#8315 = ORIENTED_EDGE ( 'NONE', *, *, #15312, .F. ) ;
#8316 = CARTESIAN_POINT ( 'NONE',  ( 19.99999999999999645, -70.29359119158495162, 15.58239511117263554 ) ) ;
#8317 = EDGE_LOOP ( 'NONE', ( #10971, #626, #11788, #16289, #20566, #17794, #9570, #11481, #9047, #3602, #3935, #13858, #14448 ) ) ;
#8318 = DIRECTION ( 'NONE',  ( -1.000000000000000000, -0.000000000000000000, 0.000000000000000000 ) ) ;
#8319 = CARTESIAN_POINT ( 'NONE',  ( 0.000000000000000000, 51.81019761368321497, 38.98425606966075918 ) ) ;
#8320 = DIRECTION ( 'NONE',  ( -1.000000000000000000, 1.202124453834178339E-10, 0.000000000000000000 ) ) ;
#8321 = EDGE_CURVE ( 'NONE', #19744, #13592, #722, .T. ) ;
#8322 = EDGE_CURVE ( 'NONE', #8201, #13929, #11583, .T. ) ;
#8323 = ORIENTED_EDGE ( 'NONE', *, *, #17713, .F. ) ;
#8324 = AXIS2_PLACEMENT_3D ( 'NONE', #15067, #860, #10402 ) ;
#8325 = DIRECTION ( 'NONE',  ( -0.000000000000000000, -0.000000000000000000, 1.000000000000000000 ) ) ;
#8326 = VERTEX_POINT ( 'NONE', #20110 ) ;
#8327 = DIRECTION ( 'NONE',  ( -1.000000000000000000, 0.000000000000000000, 0.000000000000000000 ) ) ;
#8328 = AXIS2_PLACEMENT_3D ( 'NONE', #8319, #18278, #9910 ) ;
#8329 = DIRECTION ( 'NONE',  ( 0.000000000000000000, 0.000000000000000000, 1.000000000000000000 ) ) ;
#8330 = EDGE_CURVE ( 'NONE', #10075, #13187, #7286, .T. ) ;
#8331 = ORIENTED_EDGE ( 'NONE', *, *, #15673, .T. ) ;
#8332 = CARTESIAN_POINT ( 'NONE',  ( 6.929096493489630859, -2.870125743571144472, -11.62223749981968624 ) ) ;
#8333 = VECTOR ( 'NONE', #2336, 1000.000000000000000 ) ;
#8334 = CYLINDRICAL_SURFACE ( 'NONE', #2814, 27.60000000002759535 ) ;
#8335 = APPLICATION_PROTOCOL_DEFINITION ( 'draft international standard', 'automotive_design', 1998, #7900 ) ;
#8336 = CARTESIAN_POINT ( 'NONE',  ( 16.62983158603122646, 6.888301780572504640, -14.98051249981969413 ) ) ;
#8337 = ORIENTED_EDGE ( 'NONE', *, *, #1740, .F. ) ;
#8338 = AXIS2_PLACEMENT_3D ( 'NONE', #14731, #8456, #19798 ) ;
#8339 = AXIS2_PLACEMENT_3D ( 'NONE', #15348, #15040, #16613 ) ;
#8340 = DIRECTION ( 'NONE',  ( -1.000000000000000000, 0.000000000000000000, 0.000000000000000000 ) ) ;
#8341 = DIRECTION ( 'NONE',  ( 0.000000000000000000, 0.000000000000000000, -1.000000000000000000 ) ) ;
#8342 = VECTOR ( 'NONE', #1693, 1000.000000000000000 ) ;
#8343 = VECTOR ( 'NONE', #8632, 1000.000000000000000 ) ;
#8344 = CARTESIAN_POINT ( 'NONE',  ( 13.67243654642774686, -5.663308650141536837, 1.286270581519075362 ) ) ;
#8345 = DIRECTION ( 'NONE',  ( 1.000000000000000000, 1.836909530733573776E-16, 0.000000000000000000 ) ) ;
#8346 = VERTEX_POINT ( 'NONE', #12070 ) ;
#8347 = DIRECTION ( 'NONE',  ( 0.000000000000000000, 0.000000000000000000, 1.000000000000000000 ) ) ;
#8348 = AXIS2_PLACEMENT_3D ( 'NONE', #6249, #4241, #9531 ) ;
#8349 = CARTESIAN_POINT ( 'NONE',  ( 19.99999999999999645, 43.56693332842851873, -48.57318520917461058 ) ) ;
#8350 = CARTESIAN_POINT ( 'NONE',  ( 30.45951780490842964, -42.11129053589831273, 66.34974750395082310 ) ) ;
#8351 = ORIENTED_EDGE ( 'NONE', *, *, #14218, .T. ) ;
#8352 = CARTESIAN_POINT ( 'NONE',  ( 0.000000000000000000, 0.000000000000000000, 0.000000000000000000 ) ) ;
#8353 = ORIENTED_EDGE ( 'NONE', *, *, #8639, .F. ) ;
#8354 = DIRECTION ( 'NONE',  ( -1.000000000000000000, -0.000000000000000000, -0.000000000000000000 ) ) ;
#8355 = CARTESIAN_POINT ( 'NONE',  ( 30.00000000000000000, -85.00000000000000000, -1.040949779275250179E-14 ) ) ;
#8356 = AXIS2_PLACEMENT_3D ( 'NONE', #6530, #16088, #7925 ) ;
#8357 = VERTEX_POINT ( 'NONE', #15240 ) ;
#8358 = ORIENTED_EDGE ( 'NONE', *, *, #13166, .F. ) ;
#8359 = CARTESIAN_POINT ( 'NONE',  ( 19.99999999999999645, 0.000000000000000000, 0.000000000000000000 ) ) ;
#8360 = AXIS2_PLACEMENT_3D ( 'NONE', #7713, #6106, #20726 ) ;
#8361 = CIRCLE ( 'NONE', #9055, 72.00000000007199219 ) ;
#8362 = CARTESIAN_POINT ( 'NONE',  ( 19.99999999999999645, -64.79224928664389438, -2.456263514198281150 ) ) ;
#8363 = CARTESIAN_POINT ( 'NONE',  ( 9.999999999999998224, 44.69367065308723141, -56.44887778834701919 ) ) ;
#8364 =( LENGTH_UNIT ( ) NAMED_UNIT ( * ) SI_UNIT ( .MILLI., .METRE. ) );
#8365 = DIRECTION ( 'NONE',  ( 1.000000000000000000, 0.000000000000000000, 0.000000000000000000 ) ) ;
#8366 = UNCERTAINTY_MEASURE_WITH_UNIT (LENGTH_MEASURE( 1.000000000000000082E-05 ), #2274, 'distance_accuracy_value', 'NONE');
#8367 = EDGE_CURVE ( 'NONE', #19655, #20282, #13613, .T. ) ;
#8368 = SURFACE_STYLE_USAGE ( .BOTH. , #3187 ) ;
#8369 = CARTESIAN_POINT ( 'NONE',  ( -9.015947181032835626E-10, -7.500000000000007994, 18.41995000018031803 ) ) ;
#8370 = CIRCLE ( 'NONE', #15472, 72.00000000007199219 ) ;
#8371 = CARTESIAN_POINT ( 'NONE',  ( 4.276731812588566939, -10.32494394809438809, 1.712077749713197372 ) ) ;
#8372 = CARTESIAN_POINT ( 'NONE',  ( 0.000000000000000000, 0.000000000000000000, 40.00000000000000000 ) ) ;
#8373 = CYLINDRICAL_SURFACE ( 'NONE', #11051, 27.60000000002759890 ) ;
#8374 = ORIENTED_EDGE ( 'NONE', *, *, #9135, .T. ) ;
#8375 = CARTESIAN_POINT ( 'NONE',  ( 30.00000000000000000, -85.00000000000000000, 44.99999999999999289 ) ) ;
#8376 = CARTESIAN_POINT ( 'NONE',  ( -3.580422610670018546, 18.00000000043041126, 11.23276875018031440 ) ) ;
#8377 = CARTESIAN_POINT ( 'NONE',  ( -30.00000000000000000, -164.9999999999999716, -90.00000000000001421 ) ) ;
#8378 = ORIENTED_EDGE ( 'NONE', *, *, #9777, .F. ) ;
#8379 = CARTESIAN_POINT ( 'NONE',  ( 9.999999999999998224, -64.36139404985944168, -32.27399814043940296 ) ) ;
#8380 = EDGE_LOOP ( 'NONE', ( #16202, #3359 ) ) ;
#8381 = LINE ( 'NONE', #12859, #12916 ) ;
#8382 = CARTESIAN_POINT ( 'NONE',  ( 31.53841889410551858, -36.05911901809099618, -66.76397724368483466 ) ) ;
#8383 = VERTEX_POINT ( 'NONE', #3893 ) ;
#8384 = EDGE_LOOP ( 'NONE', ( #7892, #17588, #3878, #16103 ) ) ;
#8385 = LINE ( 'NONE', #14856, #12753 ) ;
#8386 = B_SPLINE_CURVE_WITH_KNOTS ( 'NONE', 3,
 ( #17970, #13417, #161, #6614, #11401, #3342, #12131, #11812, #13614, #20387, #11907, #8627, #15203, #8736, #18491, #2173, #902, #5656, #2595, #15304, #589, #17000, #13516, #18275, #792, #20277, #19959, #9063, #7240, #3852, #20172, #10541, #10657, #2377, #2277, #15516, #7453, #8830, #12231, #5438, #3740, #4176, #13934, #17112, #7131, #13723, #3958, #7353, #5546, #18383, #5756, #7038, #10222, #20062, #13833, #10439, #682, #18598, #12022, #16901, #10328, #16684 ),
 .UNSPECIFIED., .F., .F.,
 ( 4, 2, 2, 2, 2, 2, 2, 2, 2, 2, 2, 2, 2, 2, 2, 2, 2, 2, 2, 2, 2, 2, 2, 2, 2, 2, 2, 2, 2, 2, 4 ),
 ( 4.770489558936219510E-18, 0.004535346501671356362, 0.009070693003342707519, 0.01020452962876053533, 0.01133836625417836662, 0.01360603950501402398, 0.01814138600668536994, 0.02040905925752104291, 0.02267673250835672283, 0.02494440575919239581, 0.02607824238461022362, 0.02721207901002805490, 0.03174742551169939392, 0.03401509876253507036, 0.03628277201337073987, 0.03855044526420640938, 0.03968428188962424413, 0.04081811851504207889, 0.04535346501671341790, 0.04648730164213123878, 0.04762113826754905965, 0.04988881151838471528, 0.05215648476922036397, 0.05329032139463818485, 0.05442415802005600572, 0.05895950452172729617, 0.06122717777256291710, 0.06349485102339853804, 0.06576252427423416591, 0.06803019752506979378, 0.07256554402674104953 ),
 .UNSPECIFIED. ) ;
#8387 = DIRECTION ( 'NONE',  ( 1.000000000000000000, -0.000000000000000000, 0.000000000000000000 ) ) ;
#8388 = EDGE_CURVE ( 'NONE', #4471, #5326, #10699, .T. ) ;
#8389 = CYLINDRICAL_SURFACE ( 'NONE', #8255, 65.24900000006525147 ) ;
#8390 = ORIENTED_EDGE ( 'NONE', *, *, #11328, .T. ) ;
#8391 = CARTESIAN_POINT ( 'NONE',  ( -5.303300858261583706, 5.303300859536630441, 15.68942500018031438 ) ) ;
#8392 = CARTESIAN_POINT ( 'NONE',  ( 33.27784500038035276, -116.0044176110160805, -81.92767505305181430 ) ) ;
#8393 = DIRECTION ( 'NONE',  ( 0.000000000000000000, 0.000000000000000000, 1.000000000000000000 ) ) ;
#8394 = LINE ( 'NONE', #6393, #15019 ) ;
#8395 = CARTESIAN_POINT ( 'NONE',  ( 5.200000000000002842, 0.000000000000000000, 2.500000000000000444 ) ) ;
#8396 = EDGE_CURVE ( 'NONE', #15688, #15450, #6169, .T. ) ;
#8397 = ORIENTED_EDGE ( 'NONE', *, *, #15850, .T. ) ;
#8398 = DIRECTION ( 'NONE',  ( -1.000000000000000000, -0.000000000000000000, -0.000000000000000000 ) ) ;
#8399 = ORIENTED_EDGE ( 'NONE', *, *, #19895, .T. ) ;
#8400 = CARTESIAN_POINT ( 'NONE',  ( 3.580422614997668340, 17.99999999956958519, 19.34223125018031553 ) ) ;
#8401 = DIRECTION ( 'NONE',  ( 0.000000000000000000, 0.000000000000000000, -1.000000000000000000 ) ) ;
#8402 = ORIENTED_EDGE ( 'NONE', *, *, #6712, .F. ) ;
#8403 = LINE ( 'NONE', #12788, #5178 ) ;
#8404 = VERTEX_POINT ( 'NONE', #18541 ) ;
#8405 = DIRECTION ( 'NONE',  ( -1.000000000000000000, -0.000000000000000000, -0.000000000000000000 ) ) ;
#8406 = DIRECTION ( 'NONE',  ( -1.000000000000000000, 0.000000000000000000, -0.000000000000000000 ) ) ;
#8407 = ORIENTED_EDGE ( 'NONE', *, *, #8433, .F. ) ;
#8408 = FACE_OUTER_BOUND ( 'NONE', #7086, .T. ) ;
#8409 = CARTESIAN_POINT ( 'NONE',  ( 19.99999999999999645, 0.000000000000000000, 0.000000000000000000 ) ) ;
#8410 = CARTESIAN_POINT ( 'NONE',  ( 10.00000000000000178, -164.9999999999999716, 70.00000000000000000 ) ) ;
#8411 = CARTESIAN_POINT ( 'NONE',  ( 2.222972771497741640, 11.17563879704982988, 14.43089100064742958 ) ) ;
#8412 = ORIENTED_EDGE ( 'NONE', *, *, #16669, .T. ) ;
#8413 = FACE_OUTER_BOUND ( 'NONE', #20695, .T. ) ;
#8414 = DIRECTION ( 'NONE',  ( -1.000000000000000000, 0.000000000000000000, 0.000000000000000000 ) ) ;
#8415 = VERTEX_POINT ( 'NONE', #2536 ) ;
#8416 = CARTESIAN_POINT ( 'NONE',  ( 21.45900938229203447, -1.326995226329893862, 84.99999999999998579 ) ) ;
#8417 = ADVANCED_FACE ( 'NONE', ( #17262 ), #2318, .F. ) ;
#8418 = ORIENTED_EDGE ( 'NONE', *, *, #6854, .F. ) ;
#8419 = EDGE_CURVE ( 'NONE', #5793, #19712, #9201, .T. ) ;
#8420 = CYLINDRICAL_SURFACE ( 'NONE', #4776, 4.250000000000000000 ) ;
#8421 = DIRECTION ( 'NONE',  ( -1.000000000000000000, 0.000000000000000000, 0.000000000000000000 ) ) ;
#8422 = CYLINDRICAL_SURFACE ( 'NONE', #5973, 40.00000000000000000 ) ;
#8423 = ORIENTED_EDGE ( 'NONE', *, *, #15552, .T. ) ;
#8424 = CARTESIAN_POINT ( 'NONE',  ( 5.200000000000002842, 3.306546357697854226E-16, 2.700000000000000622 ) ) ;
#8425 = EDGE_CURVE ( 'NONE', #20805, #11718, #839, .T. ) ;
#8426 = ORIENTED_EDGE ( 'NONE', *, *, #18463, .T. ) ;
#8427 = CARTESIAN_POINT ( 'NONE',  ( 19.99999999999999645, 0.000000000000000000, 0.000000000000000000 ) ) ;
#8428 = EDGE_LOOP ( 'NONE', ( #13307, #3952, #19825, #4639 ) ) ;
#8429 = CARTESIAN_POINT ( 'NONE',  ( 19.99999999999999645, 6.872116855663142232, 64.47358224882421496 ) ) ;
#8430 = CARTESIAN_POINT ( 'NONE',  ( 19.99999999999999645, -38.22257254261699444, -61.01667762370177428 ) ) ;
#8431 = DIRECTION ( 'NONE',  ( 0.9237280213470682178, 0.3830490080632377725, -1.131240564625405124E-16 ) ) ;
#8432 = CARTESIAN_POINT ( 'NONE',  ( 12.54593441764187567, 8.382925368423276069, 24.28169816884155097 ) ) ;
#8433 = EDGE_CURVE ( 'NONE', #6575, #5439, #7394, .T. ) ;
#8434 = ORIENTED_EDGE ( 'NONE', *, *, #175, .F. ) ;
#8435 = CARTESIAN_POINT ( 'NONE',  ( 19.99999999999999645, -38.69327817041739337, -52.53819777490673459 ) ) ;
#8436 = VERTEX_POINT ( 'NONE', #18636 ) ;
#8437 = DIRECTION ( 'NONE',  ( 0.000000000000000000, 0.000000000000000000, 1.000000000000000000 ) ) ;
#8438 = EDGE_CURVE ( 'NONE', #14260, #19110, #14089, .T. ) ;
#8439 = AXIS2_PLACEMENT_3D ( 'NONE', #14497, #2932, #17569 ) ;
#8440 = CARTESIAN_POINT ( 'NONE',  ( 14.79893867722909917, -2.943691928843437111, -17.85826066848093063 ) ) ;
#8441 = EDGE_CURVE ( 'NONE', #14303, #19485, #16935, .T. ) ;
#8442 = LINE ( 'NONE', #16511, #13616 ) ;
#8443 =( REPRESENTATION_RELATIONSHIP ('NONE','NONE', #13739, #20346 ) REPRESENTATION_RELATIONSHIP_WITH_TRANSFORMATION ( #3976 )SHAPE_REPRESENTATION_RELATIONSHIP( ) );
#8444 = EDGE_LOOP ( 'NONE', ( #17812, #23, #11731, #4869 ) ) ;
#8445 = ADVANCED_FACE ( 'NONE', ( #952 ), #10374, .T. ) ;
#8446 = CARTESIAN_POINT ( 'NONE',  ( -30.00000000000000000, -30.00000000000000000, -120.0000000000000142 ) ) ;
#8447 = CARTESIAN_POINT ( 'NONE',  ( 40.61263533699685979, -122.6742132524189799, -80.56091063035071898 ) ) ;
#8448 = ORIENTED_EDGE ( 'NONE', *, *, #6727, .T. ) ;
#8449 = DIRECTION ( 'NONE',  ( 0.000000000000000000, 0.000000000000000000, 1.000000000000000000 ) ) ;
#8450 = ORIENTED_EDGE ( 'NONE', *, *, #6254, .T. ) ;
#8451 = FACE_OUTER_BOUND ( 'NONE', #7954, .T. ) ;
#8452 = CARTESIAN_POINT ( 'NONE',  ( -12.72792205982779556, 12.72792206288790773, -0.9804249998196894467 ) ) ;
#8453 = ORIENTED_EDGE ( 'NONE', *, *, #14459, .F. ) ;
#8454 = ORIENTED_EDGE ( 'NONE', *, *, #18299, .T. ) ;
#8455 = DIRECTION ( 'NONE',  ( 1.000000000000000000, 0.000000000000000000, 0.000000000000000000 ) ) ;
#8456 = DIRECTION ( 'NONE',  ( -1.000000000000000000, -0.000000000000000000, -0.000000000000000000 ) ) ;
#8457 = CARTESIAN_POINT ( 'NONE',  ( -17.50000000000000355, 0.000000000000000000, 40.00000000000000000 ) ) ;
#8458 = CARTESIAN_POINT ( 'NONE',  ( -6.888301784570739272, -16.62983158437509701, 16.82886250018031049 ) ) ;
#8459 = ADVANCED_FACE ( 'NONE', ( #7496 ), #7179, .T. ) ;
#8460 = SURFACE_SIDE_STYLE ('',( #8881 ) ) ;
#8461 = CARTESIAN_POINT ( 'NONE',  ( -7.500000000000007994, 9.015942588607339023E-10, 20.77620000018031732 ) ) ;
#8462 = CARTESIAN_POINT ( 'NONE',  ( 11.17563879758427525, 2.222972768810836719, 9.075358999713197150 ) ) ;
#8463 = CARTESIAN_POINT ( 'NONE',  ( 19.99999999999999645, 0.000000000000000000, 0.000000000000000000 ) ) ;
#8464 = CARTESIAN_POINT ( 'NONE',  ( 19.99999999999999645, -44.69367065308607323, -56.44887778834792158 ) ) ;
#8465 = VERTEX_POINT ( 'NONE', #9103 ) ;
#8466 = FACE_BOUND ( 'NONE', #17455, .T. ) ;
#8467 = VECTOR ( 'NONE', #13581, 1000.000000000000000 ) ;
#8468 = CARTESIAN_POINT ( 'NONE',  ( 15.25966316918061416, -10.19618095414378622, -24.83745624981969158 ) ) ;
#8469 = DIRECTION ( 'NONE',  ( -1.000000000000000000, 0.000000000000000000, 0.000000000000000000 ) ) ;
#8470 = VERTEX_POINT ( 'NONE', #10585 ) ;
#8471 = DIRECTION ( 'NONE',  ( 0.000000000000000000, -0.000000000000000000, -1.000000000000000000 ) ) ;
#8472 = ORIENTED_EDGE ( 'NONE', *, *, #20095, .F. ) ;
#8473 = CIRCLE ( 'NONE', #2737, 2.650000000000000355 ) ;
#8474 = CARTESIAN_POINT ( 'NONE',  ( 0.000000000000000000, 0.000000000000000000, 40.00000000000000000 ) ) ;
#8475 = CARTESIAN_POINT ( 'NONE',  ( 35.04712401412363221, -25.07488921081336031, 74.50762343122646314 ) ) ;
#8476 = EDGE_CURVE ( 'NONE', #20364, #11776, #752, .T. ) ;
#8477 = EDGE_LOOP ( 'NONE', ( #14290, #11040, #4354, #1658, #3736 ) ) ;
#8478 = CIRCLE ( 'NONE', #19983, 72.00000000007199219 ) ;
#8479 = ORIENTED_EDGE ( 'NONE', *, *, #3122, .T. ) ;
#8480 = CARTESIAN_POINT ( 'NONE',  ( -30.00000000000000000, -164.9999999999999716, -90.00000000000001421 ) ) ;
#8481 = CARTESIAN_POINT ( 'NONE',  ( 19.99999999999999645, -64.79224928664393701, 2.456263514197400077 ) ) ;
#8482 = DIRECTION ( 'NONE',  ( 0.000000000000000000, 0.000000000000000000, 1.000000000000000000 ) ) ;
#8483 = CARTESIAN_POINT ( 'NONE',  ( -7.500000000179339210, -1.491842754445842800, 4.791768750180311898 ) ) ;
#8484 = CARTESIAN_POINT ( 'NONE',  ( 29.99999999999999289, -105.9516309319580927, -77.66854791982075312 ) ) ;
#8485 = CIRCLE ( 'NONE', #11214, 75.00000000000000000 ) ;
#8486 = DIRECTION ( 'NONE',  ( -1.000000000000000000, 0.000000000000000000, 0.000000000000000000 ) ) ;
#8487 = LINE ( 'NONE', #11378, #14709 ) ;
#8488 = DIRECTION ( 'NONE',  ( 0.000000000000000000, 0.000000000000000000, 1.000000000000000000 ) ) ;
#8489 = EDGE_LOOP ( 'NONE', ( #17044, #762 ) ) ;
#8490 = LINE ( 'NONE', #16658, #18330 ) ;
#8491 = ORIENTED_EDGE ( 'NONE', *, *, #7528, .T. ) ;
#8492 = DIRECTION ( 'NONE',  ( -1.000000000000000000, 0.000000000000000000, 0.000000000000000000 ) ) ;
#8493 = DIRECTION ( 'NONE',  ( -0.000000000000000000, 0.000000000000000000, 1.000000000000000000 ) ) ;
#8494 = CIRCLE ( 'NONE', #5453, 54.99999999999999289 ) ;
#8495 = VERTEX_POINT ( 'NONE', #19264 ) ;
#8496 = EDGE_CURVE ( 'NONE', #17681, #15210, #17343, .T. ) ;
#8497 = CARTESIAN_POINT ( 'NONE',  ( 5.200000000000002842, 3.306546357697854226E-16, 2.700000000000000622 ) ) ;
#8498 = ORIENTED_EDGE ( 'NONE', *, *, #7537, .T. ) ;
#8499 = CARTESIAN_POINT ( 'NONE',  ( 19.99999999999999645, -64.79224928664393701, 2.456263514197400077 ) ) ;
#8500 = LINE ( 'NONE', #17576, #11761 ) ;
#8501 = EDGE_CURVE ( 'NONE', #15340, #834, #9562, .T. ) ;
#8502 = ORIENTED_EDGE ( 'NONE', *, *, #4511, .F. ) ;
#8503 = CIRCLE ( 'NONE', #18038, 65.24900000006526568 ) ;
#8504 = VECTOR ( 'NONE', #19250, 1000.000000000000000 ) ;
#8505 = CIRCLE ( 'NONE', #7840, 7.500000000000000000 ) ;
#8506 = CARTESIAN_POINT ( 'NONE',  ( 0.000000000000000000, 0.9548212943375558037, -71.99366858485714715 ) ) ;
#8507 = CARTESIAN_POINT ( 'NONE',  ( 17.99999999999999645, -2.163824016901520184E-09, -6.871049999819689447 ) ) ;
#8508 = DIRECTION ( 'NONE',  ( 0.000000000000000000, 0.000000000000000000, -1.000000000000000000 ) ) ;
#8509 = VECTOR ( 'NONE', #15977, 1000.000000000000000 ) ;
#8510 = CARTESIAN_POINT ( 'NONE',  ( 11.17563879731705789, -1.343450868547281933E-09, 7.067609750647429578 ) ) ;
#8511 = EDGE_LOOP ( 'NONE', ( #13392, #11486, #2259, #12064 ) ) ;
#8512 = CARTESIAN_POINT ( 'NONE',  ( -2.678494666091065124, -3.072372537026387018, -5.565789719053451101 ) ) ;
#8513 = LINE ( 'NONE', #18179, #3407 ) ;
#8514 = EDGE_LOOP ( 'NONE', ( #3870, #15057, #13010, #2001 ) ) ;
#8515 = AXIS2_PLACEMENT_3D ( 'NONE', #20436, #20738, #6025 ) ;
#8516 = DIRECTION ( 'NONE',  ( 0.000000000000000000, 0.000000000000000000, 1.000000000000000000 ) ) ;
#8517 = AXIS2_PLACEMENT_3D ( 'NONE', #12109, #8920, #1310 ) ;
#8518 = ORIENTED_EDGE ( 'NONE', *, *, #17015, .F. ) ;
#8519 = CARTESIAN_POINT ( 'NONE',  ( 16.62983158603122291, 6.888301780572502864, 3.869487500180311734 ) ) ;
#8520 = DIRECTION ( 'NONE',  ( 0.000000000000000000, 0.000000000000000000, -1.000000000000000000 ) ) ;
#8521 = CARTESIAN_POINT ( 'NONE',  ( 0.000000000000000000, 0.000000000000000000, 0.000000000000000000 ) ) ;
#8522 = EDGE_LOOP ( 'NONE', ( #9035, #9511, #9070, #15038 ) ) ;
#8523 = PLANE ( 'NONE',  #14498 ) ;
#8524 = VERTEX_POINT ( 'NONE', #1274 ) ;
#8525 = DIRECTION ( 'NONE',  ( 0.000000000000000000, 0.000000000000000000, -1.000000000000000000 ) ) ;
#8526 = ORIENTED_EDGE ( 'NONE', *, *, #17670, .T. ) ;
#8527 = CARTESIAN_POINT ( 'NONE',  ( 30.00000000000000000, -42.57363661491096707, -121.3828884801879155 ) ) ;
#8528 = AXIS2_PLACEMENT_3D ( 'NONE', #6334, #16090, #3052 ) ;
#8529 = ADVANCED_FACE ( 'NONE', ( #3256 ), #19363, .F. ) ;
#8530 = AXIS2_PLACEMENT_3D ( 'NONE', #3085, #6266, #1406 ) ;
#8531 = AXIS2_PLACEMENT_3D ( 'NONE', #9638, #11432, #1688 ) ;
#8532 = EDGE_CURVE ( 'NONE', #11409, #10935, #2113, .T. ) ;
#8533 = DIRECTION ( 'NONE',  ( 1.000000000000000000, 0.000000000000000000, 0.000000000000000000 ) ) ;
#8534 = AXIS2_PLACEMENT_3D ( 'NONE', #9745, #16208, #2310 ) ;
#8535 = SHAPE_DEFINITION_REPRESENTATION ( #7115, #13064 ) ;
#8536 = CARTESIAN_POINT ( 'NONE',  ( 2.943691925285398803, -14.79893867793684059, 17.80201066884154315 ) ) ;
#8537 = ORIENTED_EDGE ( 'NONE', *, *, #9240, .F. ) ;
#8538 = DIRECTION ( 'NONE',  ( -1.000000000000000000, 0.000000000000000000, 0.000000000000000000 ) ) ;
#8539 = VECTOR ( 'NONE', #8538, 1000.000000000000000 ) ;
#8540 = EDGE_CURVE ( 'NONE', #10147, #12530, #6026, .T. ) ;
#8541 =( NAMED_UNIT ( * ) SI_UNIT ( $, .STERADIAN. ) SOLID_ANGLE_UNIT ( ) );
#8542 = CARTESIAN_POINT ( 'NONE',  ( -1.779019326032424095E-09, -14.79893867758296544, -15.79654191848093525 ) ) ;
#8543 = LINE ( 'NONE', #13853, #47 ) ;
#8544 = AXIS2_PLACEMENT_3D ( 'NONE', #19243, #3126, #12889 ) ;
#8545 = AXIS2_PLACEMENT_3D ( 'NONE', #4754, #9642, #8048 ) ;
#8546 = ORIENTED_EDGE ( 'NONE', *, *, #12672, .T. ) ;
#8547 =( GEOMETRIC_REPRESENTATION_CONTEXT ( 3 ) GLOBAL_UNCERTAINTY_ASSIGNED_CONTEXT ( ( #15356 ) ) GLOBAL_UNIT_ASSIGNED_CONTEXT ( ( #3896, #10482, #16938 ) ) REPRESENTATION_CONTEXT ( 'NONE', 'WORKASPACE' ) );
#8548 = CARTESIAN_POINT ( 'NONE',  ( 39.26462282368914458, -121.8800016488677045, 86.53530536249577665 ) ) ;
#8549 = CARTESIAN_POINT ( 'NONE',  ( -1.660531772554312280, 3.660093687634848436, -5.600000000000003197 ) ) ;
#8550 = CIRCLE ( 'NONE', #2135, 27.60000000002759535 ) ;
#8551 = B_SPLINE_CURVE_WITH_KNOTS ( 'NONE', 3,
 ( #1721, #8174, #6579, #3499, #8382, #14853, #5002, #11467, #17072, #8787, #5714, #16641, #18655, #20018, #7091, #13572, #6994, #5610 ),
 .UNSPECIFIED., .F., .F.,
 ( 4, 2, 2, 2, 2, 2, 2, 2, 4 ),
 ( 0.007425583459339141733, 0.01237513299207264328, 0.01484990775843938321, 0.01732468252480612314, 0.02722378159027312797, 0.02969855635663987137, 0.03217333112300661130, 0.03712288065574009810, 0.04702197972120707170 ),
 .UNSPECIFIED. ) ;
#8552 = ORIENTED_EDGE ( 'NONE', *, *, #15380, .F. ) ;
#8553 = DIRECTION ( 'NONE',  ( -1.000000000000000000, 0.000000000000000000, 0.000000000000000000 ) ) ;
#8554 = ORIENTED_EDGE ( 'NONE', *, *, #8676, .T. ) ;
#8555 = DIRECTION ( 'NONE',  ( 0.000000000000000000, 0.000000000000000000, -1.000000000000000000 ) ) ;
#8556 = CARTESIAN_POINT ( 'NONE',  ( 15.25966316918061239, -10.19618095414378445, 3.437543750180311442 ) ) ;
#8557 = ORIENTED_EDGE ( 'NONE', *, *, #20239, .F. ) ;
#8558 = ORIENTED_EDGE ( 'NONE', *, *, #14886, .T. ) ;
#8559 = LINE ( 'NONE', #5380, #8018 ) ;
#8560 = AXIS2_PLACEMENT_3D ( 'NONE', #12631, #11134, #3076 ) ;
#8561 = EDGE_CURVE ( 'NONE', #14529, #13850, #1681, .T. ) ;
#8562 = ADVANCED_FACE ( 'NONE', ( #9626 ), #19164, .T. ) ;
#8563 = CARTESIAN_POINT ( 'NONE',  ( 2.500000000000000000, -1.768423874527825568, -1.020999999999998575 ) ) ;
#8564 = DIRECTION ( 'NONE',  ( 1.000000000000000000, -0.000000000000000000, -0.000000000000000000 ) ) ;
#8565 = CARTESIAN_POINT ( 'NONE',  ( 2.163825119083639947E-09, 18.00000000000000355, 20.95230000018031191 ) ) ;
#8566 = CIRCLE ( 'NONE', #16348, 2.650000000000000355 ) ;
#8567 = VECTOR ( 'NONE', #20042, 1000.000000000000000 ) ;
#8568 = UNCERTAINTY_MEASURE_WITH_UNIT (LENGTH_MEASURE( 1.000000000000000082E-05 ), #8364, 'distance_accuracy_value', 'NONE');
#8570 = EDGE_CURVE ( 'NONE', #1429, #12585, #12962, .T. ) ;
#8569 = DIRECTION ( 'NONE',  ( 1.000000000000000000, 0.000000000000000000, 0.000000000000000000 ) ) ;
#8571 = CARTESIAN_POINT ( 'NONE',  ( 6.358192988180019434, 4.248408729364581582, 5.755106250180314298 ) ) ;
#8572 = CARTESIAN_POINT ( 'NONE',  ( -11.17563879704981922, 2.222972771497742972, -13.89807850028680392 ) ) ;
#8573 = AXIS2_PLACEMENT_3D ( 'NONE', #342, #3110, #13279 ) ;
#8574 = CARTESIAN_POINT ( 'NONE',  ( -2.681483223904233881, 3.070647092368428588, -5.600000000000003197 ) ) ;
#8575 = CARTESIAN_POINT ( 'NONE',  ( 0.6554360035617802227, -4.240386000424091861, -5.441324518471480687 ) ) ;
#8576 = AXIS2_PLACEMENT_3D ( 'NONE', #6232, #6123, #9207 ) ;
#8577 = CIRCLE ( 'NONE', #20434, 0.06721999999999977993 ) ;
#8578 = EDGE_LOOP ( 'NONE', ( #5739, #4623, #6997, #502 ) ) ;
#8579 = DIRECTION ( 'NONE',  ( -0.000000000000000000, -0.000000000000000000, 1.000000000000000000 ) ) ;
#8580 = CARTESIAN_POINT ( 'NONE',  ( -18.00000000000000000, 2.163826221265758884E-09, -0.2539499998196886876 ) ) ;
#8581 = CYLINDRICAL_SURFACE ( 'NONE', #3530, 49.99999999999998579 ) ;
#8582 = EDGE_CURVE ( 'NONE', #7729, #4144, #8128, .T. ) ;
#8583 = ORIENTED_EDGE ( 'NONE', *, *, #2989, .T. ) ;
#8584 = EDGE_CURVE ( 'NONE', #6966, #7729, #5829, .T. ) ;
#8585 = DIRECTION ( 'NONE',  ( 0.000000000000000000, 0.000000000000000000, -1.000000000000000000 ) ) ;
#8586 = VERTEX_POINT ( 'NONE', #4429 ) ;
#8587 = CIRCLE ( 'NONE', #4877, 2.500000000000000444 ) ;
#8588 = DIRECTION ( 'NONE',  ( 0.000000000000000000, 0.000000000000000000, 1.000000000000000000 ) ) ;
#8589 = DIRECTION ( 'NONE',  ( 0.000000000000000000, 0.000000000000000000, 1.000000000000000000 ) ) ;
#8590 = ORIENTED_EDGE ( 'NONE', *, *, #12846, .T. ) ;
#8591 = ORIENTED_EDGE ( 'NONE', *, *, #14818, .T. ) ;
#8592 = DIRECTION ( 'NONE',  ( 0.000000000000000000, 0.000000000000000000, -1.000000000000000000 ) ) ;
#8593 = EDGE_CURVE ( 'NONE', #14998, #281, #17693, .T. ) ;
#8594 = VECTOR ( 'NONE', #4595, 1000.000000000000000 ) ;
#8595 = LINE ( 'NONE', #15379, #13999 ) ;
#8596 = DIRECTION ( 'NONE',  ( 0.000000000000000000, -0.9422609221188167350, -0.3348796121709969875 ) ) ;
#8597 = AXIS2_PLACEMENT_3D ( 'NONE', #16154, #20914, #6793 ) ;
#8598 = VECTOR ( 'NONE', #8079, 1000.000000000000000 ) ;
#8599 = CARTESIAN_POINT ( 'NONE',  ( 2.870125743571137811, 6.929096493489625530, -10.81838749981969094 ) ) ;
#8600 = DIRECTION ( 'NONE',  ( 1.000000000000000000, -0.000000000000000000, -0.000000000000000000 ) ) ;
#8601 =( NAMED_UNIT ( * ) SI_UNIT ( $, .STERADIAN. ) SOLID_ANGLE_UNIT ( ) );
#8602 = CARTESIAN_POINT ( 'NONE',  ( 0.000000000000000000, 0.000000000000000000, -5.600000000000000533 ) ) ;
#8603 = DIRECTION ( 'NONE',  ( -1.000000000000000000, 0.000000000000000000, 0.000000000000000000 ) ) ;
#8604 = VERTEX_POINT ( 'NONE', #6428 ) ;
#8605 = CARTESIAN_POINT ( 'NONE',  ( 2.099999999999999645, 0.000000000000000000, -5.294516984716111097 ) ) ;
#8606 = ORIENTED_EDGE ( 'NONE', *, *, #20737, .F. ) ;
#8607 = CARTESIAN_POINT ( 'NONE',  ( -2.163827323447878234E-09, -18.00000000000000000, -4.514799999819688381 ) ) ;
#8608 = CARTESIAN_POINT ( 'NONE',  ( -1.588862400715390422, -21.45483734977870327, 70.59898835680728268 ) ) ;
#8609 = EDGE_LOOP ( 'NONE', ( #3706, #3881, #7146, #16800 ) ) ;
#8610 = DIRECTION ( 'NONE',  ( -0.000000000000000000, 0.000000000000000000, 1.000000000000000000 ) ) ;
#8611 = ORIENTED_EDGE ( 'NONE', *, *, #19095, .T. ) ;
#8612 = DIRECTION ( 'NONE',  ( -0.000000000000000000, -0.000000000000000000, -1.000000000000000000 ) ) ;
#8613 = DIRECTION ( 'NONE',  ( 0.000000000000000000, 0.000000000000000000, 1.000000000000000000 ) ) ;
#8614 = ORIENTED_EDGE ( 'NONE', *, *, #10669, .F. ) ;
#8615 = CIRCLE ( 'NONE', #5244, 2.649999999999999467 ) ;
#8616 = CARTESIAN_POINT ( 'NONE',  ( -7.500000000000000888, 1.491842755816075172, -13.46916874991221391 ) ) ;
#8617 = CARTESIAN_POINT ( 'NONE',  ( 15.25966317163202568, 10.19618095047498230, -7.754643749819691401 ) ) ;
#8618 = CARTESIAN_POINT ( 'NONE',  ( 4.924999999999924327, -8.530350227276771946, -43.00000000000000000 ) ) ;
#8619 = CYLINDRICAL_SURFACE ( 'NONE', #18409, 7.500000000000000000 ) ;
#8620 = CARTESIAN_POINT ( 'NONE',  ( 9.999999999999998224, 71.89099403602354244, 3.960426305689050075 ) ) ;
#8621 = CARTESIAN_POINT ( 'NONE',  ( 10.32494394706616347, -4.276731815070950127, 7.656672250647431177 ) ) ;
#8622 = ORIENTED_EDGE ( 'NONE', *, *, #5367, .T. ) ;
#8623 = LINE ( 'NONE', #18073, #7262 ) ;
#8624 = EDGE_CURVE ( 'NONE', #1644, #10081, #4849, .T. ) ;
#8625 = DIRECTION ( 'NONE',  ( 1.000000000000000000, 0.000000000000000000, 0.000000000000000000 ) ) ;
#8626 = VERTEX_POINT ( 'NONE', #2842 ) ;
#8627 = CARTESIAN_POINT ( 'NONE',  ( -17.67520963998171268, -12.31071423659304109, -75.43714694428801693 ) ) ;
#8628 = STYLED_ITEM ( 'NONE', ( #11600 ), #10450 ) ;
#8629 = VERTEX_POINT ( 'NONE', #6118 ) ;
#8630 = CARTESIAN_POINT ( 'NONE',  ( 18.00000000000000000, -2.163824016901520184E-09, 4.458550000180312445 ) ) ;
#8631 = CYLINDRICAL_SURFACE ( 'NONE', #9731, 27.60000000002759890 ) ;
#8632 = DIRECTION ( 'NONE',  ( -0.000000000000000000, -0.000000000000000000, -1.000000000000000000 ) ) ;
#8633 = ORIENTED_EDGE ( 'NONE', *, *, #7409, .F. ) ;
#8634 = ORIENTED_EDGE ( 'NONE', *, *, #12491, .F. ) ;
#8635 = DIRECTION ( 'NONE',  ( -1.000000000000000000, 0.000000000000000000, -0.000000000000000000 ) ) ;
#8636 = AXIS2_PLACEMENT_3D ( 'NONE', #14399, #3251, #1676 ) ;
#8637 = VERTEX_POINT ( 'NONE', #9514 ) ;
#8638 = CARTESIAN_POINT ( 'NONE',  ( 19.99999999999999645, 0.000000000000000000, 0.000000000000000000 ) ) ;
#8639 = EDGE_CURVE ( 'NONE', #2818, #19185, #11258, .T. ) ;
#8640 =( GEOMETRIC_REPRESENTATION_CONTEXT ( 3 ) GLOBAL_UNCERTAINTY_ASSIGNED_CONTEXT ( ( #8366 ) ) GLOBAL_UNIT_ASSIGNED_CONTEXT ( ( #2274, #5652, #15613 ) ) REPRESENTATION_CONTEXT ( 'NONE', 'WORKASPACE' ) );
#8641 = PRODUCT_DEFINITION_SHAPE ( 'NONE', 'NONE',  #20955 ) ;
#8642 = DIRECTION ( 'NONE',  ( -1.000000000000000000, -0.000000000000000000, -0.000000000000000000 ) ) ;
#8643 = CARTESIAN_POINT ( 'NONE',  ( -14.79893867758297610, 1.779018419858781159E-09, 11.02779191884154564 ) ) ;
#8644 = EDGE_LOOP ( 'NONE', ( #2641, #19791, #9915 ) ) ;
#8645 = EDGE_CURVE ( 'NONE', #20518, #19935, #4538, .T. ) ;
#8646 = CYLINDRICAL_SURFACE ( 'NONE', #10245, 2.649999999999993694 ) ;
#8647 = FACE_OUTER_BOUND ( 'NONE', #18624, .T. ) ;
#8648 = CARTESIAN_POINT ( 'NONE',  ( -12.54593441562640166, 8.382925371439625906, -21.98169816848092850 ) ) ;
#8649 = AXIS2_PLACEMENT_3D ( 'NONE', #5858, #15605, #377 ) ;
#8650 = DIRECTION ( 'NONE',  ( -1.000000000000000000, -0.000000000000000000, 0.000000000000000000 ) ) ;
#8651 = EDGE_CURVE ( 'NONE', #17634, #1625, #10923, .T. ) ;
#8652 = CIRCLE ( 'NONE', #3969, 65.24900000006525147 ) ;
#8653 = AXIS2_PLACEMENT_3D ( 'NONE', #18841, #1032, #17247 ) ;
#8654 = ORIENTED_EDGE ( 'NONE', *, *, #16553, .T. ) ;
#8655 = DIRECTION ( 'NONE',  ( 1.000000000000000000, 0.000000000000000000, 0.000000000000000000 ) ) ;
#8656 = CARTESIAN_POINT ( 'NONE',  ( -7.500000000000002665, 1.491842755816070509, 14.80583125008778822 ) ) ;
#8657 = VERTEX_POINT ( 'NONE', #17685 ) ;
#8658 = CARTESIAN_POINT ( 'NONE',  ( 6.358192987158596488, -4.248408730893249441, 7.522293750180316430 ) ) ;
#8659 = ORIENTED_EDGE ( 'NONE', *, *, #7603, .T. ) ;
#8660 = CYLINDRICAL_SURFACE ( 'NONE', #15960, 10.85999999999999410 ) ;
#8661 = CARTESIAN_POINT ( 'NONE',  ( -12.72792206288790950, -12.72792205982779556, 6.088325000180311086 ) ) ;
#8662 = B_SPLINE_CURVE_WITH_KNOTS ( 'NONE', 3,
 ( #17091, #20146, #13397, #8716, #5635, #4148, #14978, #12112, #20038, #7219, #19845, #15184, #16661, #3827, #12209, #15278, #18580, #5522, #5324, #2151, #18468, #8923, #18677, #11792, #10632, #13497, #8806, #8608, #18255, #2574, #7110, #15081, #7017, #7330, #19939, #4040, #15392, #10517, #10312, #661, #16974, #13590, #876, #13815, #20259, #5736, #9349, #10937, #15709, #13913, #4260, #20582, #9453, #2994, #15814, #17417, #15913, #1409, #1313, #17523, #20362, #10834 ),
 .UNSPECIFIED., .F., .F.,
 ( 4, 2, 2, 2, 2, 2, 2, 2, 2, 2, 2, 2, 2, 2, 2, 2, 2, 2, 2, 2, 2, 2, 2, 2, 2, 2, 2, 2, 2, 2, 4 ),
 ( 2.168404344971008868E-18, 0.004535346501671345953, 0.009070693003342690172, 0.01020452962876052493, 0.01133836625417835621, 0.01360603950501402572, 0.01814138600668535259, 0.02040905925752101516, 0.02267673250835667773, 0.02494440575919234376, 0.02607824238461017852, 0.02721207901002800980, 0.03174742551169934535, 0.03401509876253500098, 0.03628277201337066354, 0.03855044526420633999, 0.03968428188962416781, 0.04081811851504199562, 0.04535346501671329994, 0.04648730164213112082, 0.04762113826754894169, 0.04988881151838459038, 0.05215648476922023907, 0.05329032139463805995, 0.05442415802005587389, 0.05895950452172714351, 0.06122717777256279220, 0.06349485102339844089, 0.06576252427423409652, 0.06803019752506973827, 0.07256554402674102178 ),
 .UNSPECIFIED. ) ;
#8663 = AXIS2_PLACEMENT_3D ( 'NONE', #4087, #4736, #11696 ) ;
#8664 = ORIENTED_EDGE ( 'NONE', *, *, #11013, .T. ) ;
#8665 = ORIENTED_EDGE ( 'NONE', *, *, #8053, .T. ) ;
#8666 = DIRECTION ( 'NONE',  ( 0.000000000000000000, 0.000000000000000000, 1.000000000000000000 ) ) ;
#8667 = CIRCLE ( 'NONE', #2921, 2.500000000000002220 ) ;
#8668 = DIRECTION ( 'NONE',  ( 0.000000000000000000, 0.000000000000000000, 1.000000000000000000 ) ) ;
#8669 = FACE_OUTER_BOUND ( 'NONE', #3416, .T. ) ;
#8670 = AXIS2_PLACEMENT_3D ( 'NONE', #4808, #11079, #9273 ) ;
#8671 = AXIS2_PLACEMENT_3D ( 'NONE', #15961, #14074, #17462 ) ;
#8672 =( GEOMETRIC_REPRESENTATION_CONTEXT ( 3 ) GLOBAL_UNCERTAINTY_ASSIGNED_CONTEXT ( ( #8773 ) ) GLOBAL_UNIT_ASSIGNED_CONTEXT ( ( #10725, #18660, #12938 ) ) REPRESENTATION_CONTEXT ( 'NONE', 'WORKASPACE' ) );
#8673 = CARTESIAN_POINT ( 'NONE',  ( -30.00000000000000000, -42.57363661491096707, 121.3828884801879155 ) ) ;
#8674 = CARTESIAN_POINT ( 'NONE',  ( -5.303300859536636658, -5.303300858261589035, 0.7480750001803149196 ) ) ;
#8675 = CARTESIAN_POINT ( 'NONE',  ( 11.17563879704981566, -2.222972771497744304, -9.185578500286805337 ) ) ;
#8676 = EDGE_CURVE ( 'NONE', #11554, #9763, #3019, .T. ) ;
#8677 = VECTOR ( 'NONE', #11667, 1000.000000000000000 ) ;
#8678 = CYLINDRICAL_SURFACE ( 'NONE', #6666, 75.00000000000000000 ) ;
#8679 = DIRECTION ( 'NONE',  ( 1.000000000000000000, 0.000000000000000000, 0.000000000000000000 ) ) ;
#8680 = ADVANCED_FACE ( 'NONE', ( #14406 ), #1581, .F. ) ;
#8681 = EDGE_LOOP ( 'NONE', ( #5822, #801, #11916, #14768, #3725, #11533, #13025, #9964 ) ) ;
#8682 = DIRECTION ( 'NONE',  ( -1.000000000000000000, 0.000000000000000000, 0.000000000000000000 ) ) ;
#8683 = CIRCLE ( 'NONE', #9367, 72.00000000007199219 ) ;
#8684 = EDGE_CURVE ( 'NONE', #1182, #17144, #12283, .T. ) ;
#8685 = CARTESIAN_POINT ( 'NONE',  ( 15.25966317163202746, 10.19618095047498407, 3.574956250180310935 ) ) ;
#8686 = DIRECTION ( 'NONE',  ( -1.000000000000000000, -0.000000000000000000, -0.000000000000000000 ) ) ;
#8687 = ORIENTED_EDGE ( 'NONE', *, *, #11678, .T. ) ;
#8688 = CYLINDRICAL_SURFACE ( 'NONE', #12946, 54.99999999999999289 ) ;
#8689 = AXIS2_PLACEMENT_3D ( 'NONE', #6958, #7165, #19896 ) ;
#8690 = ORIENTED_EDGE ( 'NONE', *, *, #1444, .F. ) ;
#8691 = DIRECTION ( 'NONE',  ( 0.000000000000000000, 0.000000000000000000, 1.000000000000000000 ) ) ;
#8692 = DIRECTION ( 'NONE',  ( -1.000000000000000000, 0.000000000000000000, 0.000000000000000000 ) ) ;
#8693 = AXIS2_PLACEMENT_3D ( 'NONE', #11655, #8265, #215 ) ;
#8694 = EDGE_CURVE ( 'NONE', #18360, #10009, #6523, .T. ) ;
#8695 = EDGE_LOOP ( 'NONE', ( #12892, #549, #10815, #17809, #9893 ) ) ;
#8696 = ADVANCED_FACE ( 'NONE', ( #6735 ), #11510, .F. ) ;
#8697 = VERTEX_POINT ( 'NONE', #10238 ) ;
#8698 = CARTESIAN_POINT ( 'NONE',  ( 0.000000000000000000, 0.000000000000000000, 129.0000000000000000 ) ) ;
#8699 = DIRECTION ( 'NONE',  ( 0.000000000000000000, -0.000000000000000000, -1.000000000000000000 ) ) ;
#8700 = AXIS2_PLACEMENT_3D ( 'NONE', #8527, #5670, #604 ) ;
#8701 = DIRECTION ( 'NONE',  ( 1.000000000000000000, 0.000000000000000000, 0.000000000000000000 ) ) ;
#8702 = EDGE_CURVE ( 'NONE', #8788, #10906, #13986, .T. ) ;
#8703 = AXIS2_PLACEMENT_3D ( 'NONE', #7295, #18547, #12284 ) ;
#8704 = CARTESIAN_POINT ( 'NONE',  ( 4.248408730893245888, 6.358192987158590270, -10.52385624981969059 ) ) ;
#8705 = CIRCLE ( 'NONE', #9353, 2.500000000000000444 ) ;
#8706 = DIRECTION ( 'NONE',  ( -1.000000000000000000, -0.000000000000000000, -0.000000000000000000 ) ) ;
#8707 = PRESENTATION_STYLE_ASSIGNMENT (( #13176 ) ) ;
#8708 = DIRECTION ( 'NONE',  ( 1.000000000000000000, -0.000000000000000000, -0.000000000000000000 ) ) ;
#8709 = CARTESIAN_POINT ( 'NONE',  ( 30.00000000000000000, -29.99999999999999645, -45.00000000000000000 ) ) ;
#8710 = EDGE_CURVE ( 'NONE', #11468, #13959, #6837, .T. ) ;
#8711 = ORIENTED_EDGE ( 'NONE', *, *, #16603, .T. ) ;
#8712 = CARTESIAN_POINT ( 'NONE',  ( 7.500000000000007994, 1.491842754878805577, 6.344168750087792574 ) ) ;
#8713 = EDGE_CURVE ( 'NONE', #17642, #14849, #12632, .T. ) ;
#8714 = VERTEX_POINT ( 'NONE', #3356 ) ;
#8715 = CARTESIAN_POINT ( 'NONE',  ( 12.72792205982779734, -12.72792206288791128, -5.692924999819687137 ) ) ;
#8716 = CARTESIAN_POINT ( 'NONE',  ( -20.80121494421294415, -5.547499958777468265, 80.68520720011532887 ) ) ;
#8717 = VECTOR ( 'NONE', #6324, 1000.000000000000114 ) ;
#8718 = EDGE_LOOP ( 'NONE', ( #17413, #13145, #2068, #12130 ) ) ;
#8719 = DIRECTION ( 'NONE',  ( -1.000000000000000000, -0.000000000000000000, -0.000000000000000000 ) ) ;
#8720 = ORIENTED_EDGE ( 'NONE', *, *, #14277, .F. ) ;
#8721 = EDGE_CURVE ( 'NONE', #4150, #4451, #18376, .T. ) ;
#8722 = CARTESIAN_POINT ( 'NONE',  ( -31.75000000000000000, -10.85999999999999410, 1.329966423874024955E-15 ) ) ;
#8723 = DIRECTION ( 'NONE',  ( -1.000000000000000000, 0.000000000000000000, 0.000000000000000000 ) ) ;
#8724 = AXIS2_PLACEMENT_3D ( 'NONE', #8749, #15215, #696 ) ;
#8725 =( BOUNDED_CURVE ( )  B_SPLINE_CURVE ( 2, ( #19359, #4844, #9814, #11315, #3252, #1677, #14597, #72, #6528, #19464, #1008, #12349, #12669, #10855, #7777, #2596, #14252 ),
 .UNSPECIFIED., .F., .F. ) 
 B_SPLINE_CURVE_WITH_KNOTS ( ( 3, 2, 2, 2, 2, 2, 2, 2, 3 ),
 ( 0.6000000000038511194, 0.6125000000038511860, 0.6250000000038511416, 0.6375000000038510972, 0.6500000000038511638, 0.6625000000038511194, 0.6750000000038511860, 0.6875000000038511416, 0.7000000000038510972 ),
 .UNSPECIFIED. ) 
 CURVE ( )  GEOMETRIC_REPRESENTATION_ITEM ( )  RATIONAL_B_SPLINE_CURVE ( ( 0.9999999999940800688, 0.9807852804091503618, 1.000000000000000000, 0.9807852804032304306, 1.000000000000000000, 0.9807852804032304306, 1.000000000000000000, 0.9807852804032304306, 1.000000000000000000, 0.9807852804032304306, 1.000000000000000000, 0.9807852804032304306, 1.000000000000000000, 0.9807852804032304306, 1.000000000000000000, 0.9807852803973104994, 1.000000000005919931 ) ) 
 REPRESENTATION_ITEM ( '' )  );
#8726 = ORIENTED_EDGE ( 'NONE', *, *, #8885, .T. ) ;
#8727 = CARTESIAN_POINT ( 'NONE',  ( -2.870125741905210415, 6.929096494179677990, -11.99651249981969414 ) ) ;
#8728 = CARTESIAN_POINT ( 'NONE',  ( 12.72792205982779379, -12.72792206288790950, -15.11792499981969051 ) ) ;
#8729 = CARTESIAN_POINT ( 'NONE',  ( -4.000000000000000000, 0.000000000000000000, 0.000000000000000000 ) ) ;
#8730 = DIRECTION ( 'NONE',  ( 1.000000000000000000, 0.000000000000000000, 0.000000000000000000 ) ) ;
#8731 = CARTESIAN_POINT ( 'NONE',  ( -2.222972771497745192, -11.17563879704982632, 9.718391000647429223 ) ) ;
#8732 = ORIENTED_EDGE ( 'NONE', *, *, #16961, .T. ) ;
#8733 = ADVANCED_FACE ( 'NONE', ( #499 ), #179, .F. ) ;
#8734 = CARTESIAN_POINT ( 'NONE',  ( -17.50000000000000355, 0.000000000000000000, 43.00000000000000000 ) ) ;
#8735 = VERTEX_POINT ( 'NONE', #6948 ) ;
#8736 = CARTESIAN_POINT ( 'NONE',  ( -15.44968093174340140, -14.96845338175448781, -73.80849194119340950 ) ) ;
#8737 = ORIENTED_EDGE ( 'NONE', *, *, #3770, .F. ) ;
#8738 = CARTESIAN_POINT ( 'NONE',  ( 17.99999999956958163, -3.580422614997676334, 14.17808125018031440 ) ) ;
#8739 = CARTESIAN_POINT ( 'NONE',  ( 4.925000000000044231, 8.530350227276702668, -40.00000000000000000 ) ) ;
#8740 = CYLINDRICAL_SURFACE ( 'NONE', #227, 27.60000000002759535 ) ;
#8741 = VERTEX_POINT ( 'NONE', #8430 ) ;
#8742 = CARTESIAN_POINT ( 'NONE',  ( 9.999999999999998224, -29.55812890831937167, -65.65300461859717984 ) ) ;
#8743 = ORIENTED_EDGE ( 'NONE', *, *, #6372, .F. ) ;
#8744 = CARTESIAN_POINT ( 'NONE',  ( -6.358192987158597376, 4.248408730893249441, 12.23479375018031590 ) ) ;
#8745 = ORIENTED_EDGE ( 'NONE', *, *, #4652, .T. ) ;
#8746 = CARTESIAN_POINT ( 'NONE',  ( 0.000000000000000000, 0.000000000000000000, 0.000000000000000000 ) ) ;
#8747 = EDGE_CURVE ( 'NONE', #20075, #13834, #13433, .T. ) ;
#8748 = ORIENTED_EDGE ( 'NONE', *, *, #11799, .T. ) ;
#8749 = CARTESIAN_POINT ( 'NONE',  ( 0.000000000000000000, 0.000000000000000000, 40.00000000000000000 ) ) ;
#8750 = DIRECTION ( 'NONE',  ( 0.000000000000000000, -0.9790840876823249106, 0.2034560130526240906 ) ) ;
#8751 = APPLICATION_PROTOCOL_DEFINITION ( 'draft international standard', 'automotive_design', 1998, #7078 ) ;
#8752 = CARTESIAN_POINT ( 'NONE',  ( -13.67243654642775574, 5.663308650141533285, 21.04185441884154883 ) ) ;
#8753 = ORIENTED_EDGE ( 'NONE', *, *, #4751, .T. ) ;
#8754 = CARTESIAN_POINT ( 'NONE',  ( 6.177131623262577698, 0.000000000000000000, 10.85999999999999410 ) ) ;
#8755 = CARTESIAN_POINT ( 'NONE',  ( 8.900000000000053646, 10.82531754730546147, 43.00000000000000000 ) ) ;
#8756 = CARTESIAN_POINT ( 'NONE',  ( 12.54593441562639988, -8.382925371439625906, -26.69419816848093419 ) ) ;
#8757 = CARTESIAN_POINT ( 'NONE',  ( -65.00002539999999840, 0.000000000000000000, 0.000000000000000000 ) ) ;
#8758 = VERTEX_POINT ( 'NONE', #5359 ) ;
#8759 = DIRECTION ( 'NONE',  ( -1.000000000000000000, -0.000000000000000000, 0.000000000000000000 ) ) ;
#8760 = DIRECTION ( 'NONE',  ( 1.000000000000000000, 0.000000000000000000, 0.000000000000000000 ) ) ;
#8761 = ORIENTED_EDGE ( 'NONE', *, *, #8645, .T. ) ;
#8762 = DIRECTION ( 'NONE',  ( -1.000000000000000000, 0.000000000000000000, 0.000000000000000000 ) ) ;
#8763 = ORIENTED_EDGE ( 'NONE', *, *, #17082, .T. ) ;
#8764 = LINE ( 'NONE', #12060, #13946 ) ;
#8765 = CARTESIAN_POINT ( 'NONE',  ( -16.62983158603121936, -6.888301780572499311, 6.677387500180310020 ) ) ;
#8766 = ADVANCED_FACE ( 'NONE', ( #9818 ), #11828, .T. ) ;
#8767 = EDGE_LOOP ( 'NONE', ( #19248, #4777 ) ) ;
#8768 = ORIENTED_EDGE ( 'NONE', *, *, #648, .F. ) ;
#8769 = DIRECTION ( 'NONE',  ( 0.000000000000000000, 0.000000000000000000, -1.000000000000000000 ) ) ;
#8770 = DIRECTION ( 'NONE',  ( 0.000000000000000000, 0.000000000000000000, -1.000000000000000000 ) ) ;
#8771 = CARTESIAN_POINT ( 'NONE',  ( 0.000000000000000000, 0.000000000000000000, 68.00000000000000000 ) ) ;
#8772 = CARTESIAN_POINT ( 'NONE',  ( 6.929096494179683319, 2.870125741905213079, -12.80036249981968766 ) ) ;
#8773 = UNCERTAINTY_MEASURE_WITH_UNIT (LENGTH_MEASURE( 1.000000000000000082E-05 ), #10725, 'distance_accuracy_value', 'NONE');
#8774 = FACE_OUTER_BOUND ( 'NONE', #7114, .T. ) ;
#8775 = CARTESIAN_POINT ( 'NONE',  ( 1.491842754445843688, -7.500000000179346316, -0.7245812498196841922 ) ) ;
#8776 = DIRECTION ( 'NONE',  ( 1.000000000000000000, 0.000000000000000000, -0.000000000000000000 ) ) ;
#8777 = CARTESIAN_POINT ( 'NONE',  ( 10.32494394706615637, -4.276731815070946574, -8.891047250286803205 ) ) ;
#8778 = CARTESIAN_POINT ( 'NONE',  ( 0.000000000000000000, 58.26603306962022089, -42.29739224042413781 ) ) ;
#8779 = EDGE_LOOP ( 'NONE', ( #13623, #15817, #7253, #18379 ) ) ;
#8780 = DIRECTION ( 'NONE',  ( 1.000000000000000000, 1.836909530733573776E-16, 0.000000000000000000 ) ) ;
#8781 = CARTESIAN_POINT ( 'NONE',  ( 16.62983158603122291, 6.888301780572502864, -5.555512499819688088 ) ) ;
#8782 = DIRECTION ( 'NONE',  ( -1.000000000000000000, -0.000000000000000000, -0.000000000000000000 ) ) ;
#8783 = VERTEX_POINT ( 'NONE', #18093 ) ;
#8784 = CARTESIAN_POINT ( 'NONE',  ( 0.000000000000000000, 0.000000000000000000, 0.000000000000000000 ) ) ;
#8785 = ORIENTED_EDGE ( 'NONE', *, *, #10809, .F. ) ;
#8786 = DIRECTION ( 'NONE',  ( -1.000000000000000000, -0.000000000000000000, -0.000000000000000000 ) ) ;
#8787 = CARTESIAN_POINT ( 'NONE',  ( 35.95678405163886282, -23.08991427661194606, -69.94389397731961822 ) ) ;
#8788 = VERTEX_POINT ( 'NONE', #6531 ) ;
#8789 = ORIENTED_EDGE ( 'NONE', *, *, #18227, .T. ) ;
#8790 = FACE_OUTER_BOUND ( 'NONE', #13197, .T. ) ;
#8791 = CARTESIAN_POINT ( 'NONE',  ( 50.00000000000000000, -164.9999999999999716, 90.00000000000001421 ) ) ;
#8792 = EDGE_CURVE ( 'NONE', #17353, #9919, #9246, .T. ) ;
#8793 = EDGE_CURVE ( 'NONE', #13722, #11488, #16390, .T. ) ;
#8794 = CYLINDRICAL_SURFACE ( 'NONE', #20087, 2.649999999999998579 ) ;
#8795 = CARTESIAN_POINT ( 'NONE',  ( -4.248408730893245000, -6.358192987158590270, -15.23635624981969272 ) ) ;
#8796 = AXIS2_PLACEMENT_3D ( 'NONE', #19127, #8188, #9471 ) ;
#8797 = CARTESIAN_POINT ( 'NONE',  ( 6.249999999999902300, -10.82531754730554496, 43.00000000000000000 ) ) ;
#8798 = EDGE_CURVE ( 'NONE', #9320, #2408, #18717, .T. ) ;
#8799 = CARTESIAN_POINT ( 'NONE',  ( 0.000000000000000000, -6.872116855662673274, -64.47358224882424338 ) ) ;
#8800 = CARTESIAN_POINT ( 'NONE',  ( 9.999999999999998224, -51.96384592647235934, 49.83732252579596889 ) ) ;
#8801 = DIRECTION ( 'NONE',  ( 1.000000000000000000, 0.000000000000000000, 0.000000000000000000 ) ) ;
#8802 = VERTEX_POINT ( 'NONE', #17894 ) ;
#8803 = DIRECTION ( 'NONE',  ( 0.000000000000000000, 1.000000000000000000, 1.541976423090495387E-16 ) ) ;
#8804 = EDGE_LOOP ( 'NONE', ( #14233, #5043, #8789, #16723 ) ) ;
#8805 = CARTESIAN_POINT ( 'NONE',  ( -17.99999999956958519, 3.580422614997674113, 7.560981250180312863 ) ) ;
#8806 = CARTESIAN_POINT ( 'NONE',  ( -3.108800563652534432, -21.28778730843814060, 70.66877985699922249 ) ) ;
#8807 = AXIS2_PLACEMENT_3D ( 'NONE', #18061, #3527, #14983 ) ;
#8808 = VERTEX_POINT ( 'NONE', #10035 ) ;
#8809 = DIRECTION ( 'NONE',  ( 0.000000000000000000, -1.541976423090495387E-16, 1.000000000000000000 ) ) ;
#8810 = ORIENTED_EDGE ( 'NONE', *, *, #19834, .T. ) ;
#8811 = PRODUCT ( 'needle roller bearing_nh_iso_ISO 3245 - 1532D - 14,SI,NC,14', 'needle roller bearing_nh_iso_ISO 3245 - 1532D - 14,SI,NC,14', '', ( #3665 ) ) ;
#8812 = DIRECTION ( 'NONE',  ( 0.000000000000000000, 0.000000000000000000, 1.000000000000000000 ) ) ;
#8813 = CARTESIAN_POINT ( 'NONE',  ( 20.00000000000000355, 0.000000000000000000, 0.000000000000000000 ) ) ;
#8814 = ORIENTED_EDGE ( 'NONE', *, *, #11594, .F. ) ;
#8815 = DIRECTION ( 'NONE',  ( -1.000000000000000000, 0.000000000000000000, 0.000000000000000000 ) ) ;
#8816 = ADVANCED_FACE ( 'NONE', ( #3558 ), #8229, .T. ) ;
#8817 = CARTESIAN_POINT ( 'NONE',  ( 0.000000000000000000, 42.42902769288536291, 49.02903636734212967 ) ) ;
#8818 = CARTESIAN_POINT ( 'NONE',  ( -15.25966316918061416, 10.19618095414378445, -1.274956249819690024 ) ) ;
#8819 = CARTESIAN_POINT ( 'NONE',  ( 30.00000000000000000, -47.50729195424787576, -66.54687817268471406 ) ) ;
#8820 = ADVANCED_FACE ( 'NONE', ( #9921 ), #8334, .T. ) ;
#8821 = EDGE_CURVE ( 'NONE', #5556, #10438, #14647, .T. ) ;
#8822 = CARTESIAN_POINT ( 'NONE',  ( -6.358192988180015881, -4.248408729364577141, 13.62770625018031012 ) ) ;
#8823 = CIRCLE ( 'NONE', #10534, 72.00000000007199219 ) ;
#8824 = CARTESIAN_POINT ( 'NONE',  ( 6.330490856366294494, -9.474249098604513364, -0.8847339993525716872 ) ) ;
#8825 = ORIENTED_EDGE ( 'NONE', *, *, #16526, .F. ) ;
#8826 = CARTESIAN_POINT ( 'NONE',  ( 6.249999999999902300, -10.82531754730554496, 126.0000000000000000 ) ) ;
#8827 = ADVANCED_FACE ( 'NONE', ( #10347 ), #4195, .F. ) ;
#8828 = FACE_OUTER_BOUND ( 'NONE', #10451, .T. ) ;
#8829 = VERTEX_POINT ( 'NONE', #13633 ) ;
#8830 = CARTESIAN_POINT ( 'NONE',  ( 9.140901424055394742, -19.46372757881361792, -71.47335990888088020 ) ) ;
#8831 = ORIENTED_EDGE ( 'NONE', *, *, #2561, .T. ) ;
#8832 = CARTESIAN_POINT ( 'NONE',  ( -2.163827323447878234E-09, -18.00000000000000000, 6.814800000180313511 ) ) ;
#8833 = DIRECTION ( 'NONE',  ( -1.000000000000000000, 0.000000000000000000, 0.000000000000000000 ) ) ;
#8834 = DIRECTION ( 'NONE',  ( -1.000000000000000000, -0.000000000000000000, 0.000000000000000000 ) ) ;
#8835 =( BOUNDED_CURVE ( )  B_SPLINE_CURVE ( 2, ( #13221, #20853, #3360, #11213, #10040, #11429, #18097, #290, #17898, #9823, #19671, #3458, #14062, #16290, #17988, #9925, #14713 ),
 .UNSPECIFIED., .F., .F. ) 
 B_SPLINE_CURVE_WITH_KNOTS ( ( 3, 2, 2, 2, 2, 2, 2, 2, 3 ),
 ( 0.2000000000038511805, 0.2125000000038511638, 0.2250000000038511749, 0.2375000000038511860, 0.2500000000038511971, 0.2625000000038512082, 0.2750000000038512193, 0.2875000000038511749, 0.3000000000038511860 ),
 .UNSPECIFIED. ) 
 CURVE ( )  GEOMETRIC_REPRESENTATION_ITEM ( )  RATIONAL_B_SPLINE_CURVE ( ( 0.9999999999940800688, 0.9807852804091503618, 1.000000000000000000, 0.9807852804032304306, 1.000000000000000000, 0.9807852804032304306, 1.000000000000000000, 0.9807852804032304306, 1.000000000000000000, 0.9807852804032304306, 1.000000000000000000, 0.9807852804032304306, 1.000000000000000000, 0.9807852804032304306, 1.000000000000000000, 0.9807852803973104994, 1.000000000005919931 ) ) 
 REPRESENTATION_ITEM ( '' )  );
#8836 = ORIENTED_EDGE ( 'NONE', *, *, #2211, .T. ) ;
#8837 = AXIS2_PLACEMENT_3D ( 'NONE', #9476, #16352, #9581 ) ;
#8838 = CYLINDRICAL_SURFACE ( 'NONE', #10594, 27.60000000002760245 ) ;
#8839 = ORIENTED_EDGE ( 'NONE', *, *, #14857, .T. ) ;
#8840 = DIRECTION ( 'NONE',  ( 0.000000000000000000, 0.000000000000000000, -1.000000000000000000 ) ) ;
#8841 = VECTOR ( 'NONE', #10472, 1000.000000000000000 ) ;
#8842 = EDGE_CURVE ( 'NONE', #540, #13080, #13951, .T. ) ;
#8843 = ORIENTED_EDGE ( 'NONE', *, *, #1359, .F. ) ;
#8844 = CARTESIAN_POINT ( 'NONE',  ( 0.000000000000000000, 0.000000000000000000, 68.00000000000000000 ) ) ;
#8845 = EDGE_CURVE ( 'NONE', #6733, #9385, #3146, .T. ) ;
#8846 = EDGE_CURVE ( 'NONE', #9221, #16803, #12365, .T. ) ;
#8847 = AXIS2_PLACEMENT_3D ( 'NONE', #7391, #13977, #5798 ) ;
#8848 = CARTESIAN_POINT ( 'NONE',  ( 3.344563996438205677, 2.687817229851463097, -5.441324518471517102 ) ) ;
#8849 = EDGE_CURVE ( 'NONE', #20286, #19852, #17017, .T. ) ;
#8850 = CARTESIAN_POINT ( 'NONE',  ( 24.99999999999999645, -99.99999999999998579, 52.00000000000000000 ) ) ;
#8851 = ITEM_DEFINED_TRANSFORMATION ( 'NONE', 'NONE', #9971,  #12461 ) ;
#8852 = CARTESIAN_POINT ( 'NONE',  ( -14.79893867793684059, -2.943691925285399691, 10.73326066884154528 ) ) ;
#8853 = AXIS2_PLACEMENT_3D ( 'NONE', #14168, #3023, #15742 ) ;
#8855 = EDGE_LOOP ( 'NONE', ( #10579, #17597 ) ) ;
#8854 = AXIS2_PLACEMENT_3D ( 'NONE', #10196, #10309, #15078 ) ;
#8856 = CARTESIAN_POINT ( 'NONE',  ( 19.99999999999999645, 0.000000000000000000, 0.000000000000000000 ) ) ;
#8857 = AXIS2_PLACEMENT_3D ( 'NONE', #15479, #1291, #4349 ) ;
#8858 = ORIENTED_EDGE ( 'NONE', *, *, #4880, .T. ) ;
#8859 = CARTESIAN_POINT ( 'NONE',  ( 19.99999999999999645, 14.55863677812212131, -63.60407295269091321 ) ) ;
#8860 = CARTESIAN_POINT ( 'NONE',  ( 14.79893867722909917, -2.943691928843437111, -27.28326066848093490 ) ) ;
#8861 = DIRECTION ( 'NONE',  ( -1.000000000000000000, 0.000000000000000000, 0.000000000000000000 ) ) ;
#8862 = VERTEX_POINT ( 'NONE', #20289 ) ;
#8863 = CARTESIAN_POINT ( 'NONE',  ( 33.76967208201212145, -116.6944083555470826, 82.37802687633472942 ) ) ;
#8864 = FACE_OUTER_BOUND ( 'NONE', #5340, .T. ) ;
#8865 = ORIENTED_EDGE ( 'NONE', *, *, #1832, .F. ) ;
#8866 = AXIS2_PLACEMENT_3D ( 'NONE', #15144, #15043, #11851 ) ;
#8867 = CARTESIAN_POINT ( 'NONE',  ( 3.868535272439428407, -22.67561597872231616, -75.51271470091462845 ) ) ;
#8868 = ORIENTED_EDGE ( 'NONE', *, *, #18120, .F. ) ;
#8869 = DIRECTION ( 'NONE',  ( 0.000000000000000000, 0.000000000000000000, 1.000000000000000000 ) ) ;
#8870 = CARTESIAN_POINT ( 'NONE',  ( -10.19618095047497874, 15.25966317163202746, 8.739106250180309843 ) ) ;
#8871 = AXIS2_PLACEMENT_3D ( 'NONE', #3768, #615, #3984 ) ;
#8872 = EDGE_LOOP ( 'NONE', ( #16926, #10022 ) ) ;
#8873 = AXIS2_PLACEMENT_3D ( 'NONE', #12729, #14317, #20759 ) ;
#8874 = VERTEX_POINT ( 'NONE', #20406 ) ;
#8875 = CYLINDRICAL_SURFACE ( 'NONE', #1255, 72.00000000007199219 ) ;
#8876 = DIRECTION ( 'NONE',  ( -1.000000000000000000, -0.000000000000000000, -0.000000000000000000 ) ) ;
#8877 = CARTESIAN_POINT ( 'NONE',  ( 19.99999999999999645, 36.54710069451126486, -54.05313526368077248 ) ) ;
#8878 = PRESENTATION_STYLE_ASSIGNMENT (( #10586 ) ) ;
#8879 = AXIS2_PLACEMENT_3D ( 'NONE', #15751, #12252, #9401 ) ;
#8880 = CARTESIAN_POINT ( 'NONE',  ( -17.99999999956958874, 3.580422614997675002, 18.89058125018030765 ) ) ;
#8881 = SURFACE_STYLE_FILL_AREA ( #5593 ) ;
#8882 = CARTESIAN_POINT ( 'NONE',  ( -2.870125741905213079, 6.929096494179683319, -5.731612499819686235 ) ) ;
#8883 = VECTOR ( 'NONE', #2954, 1000.000000000000000 ) ;
#8884 = CARTESIAN_POINT ( 'NONE',  ( 5.303300858261588147, -5.303300859536636658, 17.24182500018031661 ) ) ;
#8885 = EDGE_CURVE ( 'NONE', #10995, #10075, #442, .T. ) ;
#8886 = AXIS2_PLACEMENT_3D ( 'NONE', #1692, #19272, #3169 ) ;
#8887 = CARTESIAN_POINT ( 'NONE',  ( 7.902369976724389566, -7.902369978624323110, -8.301984750286806047 ) ) ;
#8888 = CIRCLE ( 'NONE', #14329, 27.60000000002759535 ) ;
#8889 = EDGE_CURVE ( 'NONE', #8465, #11004, #8964, .T. ) ;
#8890 = B_SPLINE_CURVE_WITH_KNOTS ( 'NONE', 3,
 ( #15228, #8549, #5372, #12056, #3988, #7166 ),
 .UNSPECIFIED., .F., .F.,
 ( 4, 2, 4 ),
 ( 0.002336974151641539946, 0.003500975885716448889, 0.004664977619791357832 ),
 .UNSPECIFIED. ) ;
#8891 = AXIS2_PLACEMENT_3D ( 'NONE', #3575, #16830, #19898 ) ;
#8892 = CARTESIAN_POINT ( 'NONE',  ( -52.49999999999999289, -120.0000000000000142, 5.000000000000000000 ) ) ;
#8893 = ORIENTED_EDGE ( 'NONE', *, *, #20402, .F. ) ;
#8894 = DIRECTION ( 'NONE',  ( 0.000000000000000000, 0.000000000000000000, 1.000000000000000000 ) ) ;
#8895 = CARTESIAN_POINT ( 'NONE',  ( -17.99999999956958519, 3.580422614997674113, -9.384418749819685601 ) ) ;
#8896 = FACE_BOUND ( 'NONE', #14505, .T. ) ;
#8897 = ORIENTED_EDGE ( 'NONE', *, *, #6796, .T. ) ;
#8898 = CYLINDRICAL_SURFACE ( 'NONE', #7512, 72.00000000007199219 ) ;
#8899 = VERTEX_POINT ( 'NONE', #13737 ) ;
#8900 = DIRECTION ( 'NONE',  ( 0.000000000000000000, 0.000000000000000000, -1.000000000000000000 ) ) ;
#8901 = DIRECTION ( 'NONE',  ( 1.000000000000000000, 0.000000000000000000, -0.000000000000000000 ) ) ;
#8902 = VERTEX_POINT ( 'NONE', #2709 ) ;
#8903 = EDGE_LOOP ( 'NONE', ( #16245, #3912, #19509, #1184 ) ) ;
#8904 = CARTESIAN_POINT ( 'NONE',  ( -8.500000000000000000, 1.040949779275250140E-15, 90.00000000000000000 ) ) ;
#8905 = VECTOR ( 'NONE', #13093, 1000.000000000000000 ) ;
#8906 = AXIS2_PLACEMENT_3D ( 'NONE', #14373, #9072, #1016 ) ;
#8907 = EDGE_CURVE ( 'NONE', #20839, #16808, #18721, .T. ) ;
#8908 = CARTESIAN_POINT ( 'NONE',  ( -18.00000000000000000, 2.204364238465235428E-15, -130.0000000000000000 ) ) ;
#8909 = DIRECTION ( 'NONE',  ( 0.000000000000000000, 0.000000000000000000, 1.000000000000000000 ) ) ;
#8910 = AXIS2_PLACEMENT_3D ( 'NONE', #1770, #19259, #8124 ) ;
#8911 = CIRCLE ( 'NONE', #13314, 50.00000000000001421 ) ;
#8912 = CARTESIAN_POINT ( 'NONE',  ( -2.870125743571140919, -6.929096493489624642, -6.105887499819689701 ) ) ;
#8913 = ADVANCED_FACE ( 'NONE', ( #699 ), #20192, .F. ) ;
#8914 = CARTESIAN_POINT ( 'NONE',  ( 93.70999227554992217, -50.00000000000000000, -90.00000000000001421 ) ) ;
#8915 = DIRECTION ( 'NONE',  ( 0.000000000000000000, 0.000000000000000000, 1.000000000000000000 ) ) ;
#8916 = CARTESIAN_POINT ( 'NONE',  ( 50.00000000000000000, -105.0000000000000000, -90.00000000000001421 ) ) ;
#8917 = DIRECTION ( 'NONE',  ( 1.000000000000000000, -0.000000000000000000, -0.000000000000000000 ) ) ;
#8918 = CIRCLE ( 'NONE', #16365, 2.099999999999997868 ) ;
#8919 = ORIENTED_EDGE ( 'NONE', *, *, #10693, .F. ) ;
#8920 = DIRECTION ( 'NONE',  ( -1.000000000000000000, -0.000000000000000000, -0.000000000000000000 ) ) ;
#8921 = ORIENTED_EDGE ( 'NONE', *, *, #14150, .F. ) ;
#8922 = CARTESIAN_POINT ( 'NONE',  ( -15.25966317163203279, -10.19618095047498052, -3.042143749819686160 ) ) ;
#8923 = CARTESIAN_POINT ( 'NONE',  ( -9.587454675490707956, -19.24766271911509463, 71.57389447320451836 ) ) ;
#8924 = ORIENTED_EDGE ( 'NONE', *, *, #10272, .F. ) ;
#8925 = EDGE_CURVE ( 'NONE', #4757, #10860, #10673, .T. ) ;
#8926 = DIRECTION ( 'NONE',  ( -1.000000000000000000, -0.000000000000000000, -0.000000000000000000 ) ) ;
#8927 = ORIENTED_EDGE ( 'NONE', *, *, #10493, .T. ) ;
#8928 = FACE_OUTER_BOUND ( 'NONE', #9369, .T. ) ;
#8929 = CARTESIAN_POINT ( 'NONE',  ( 19.74873734152915716, 24.74873734152916072, -130.0000000000000000 ) ) ;
#8930 = DIRECTION ( 'NONE',  ( 1.000000000000000000, 0.000000000000000000, 0.000000000000000000 ) ) ;
#8931 = AXIS2_PLACEMENT_3D ( 'NONE', #1840, #17641, #246 ) ;
#8932 = VERTEX_POINT ( 'NONE', #12040 ) ;
#8933 = DIRECTION ( 'NONE',  ( 0.000000000000000000, -0.8660254037844390407, -0.4999999999999993339 ) ) ;
#8934 = AXIS2_PLACEMENT_3D ( 'NONE', #1509, #16220, #10064 ) ;
#8935 = DIRECTION ( 'NONE',  ( 1.000000000000000000, 0.000000000000000000, 0.000000000000000000 ) ) ;
#8936 = CARTESIAN_POINT ( 'NONE',  ( -16.62983158603121936, -6.888301780572499311, -12.17261249981969229 ) ) ;
#8937 = AXIS2_PLACEMENT_3D ( 'NONE', #13803, #20250, #553 ) ;
#8938 = FACE_OUTER_BOUND ( 'NONE', #2411, .T. ) ;
#8939 = ADVANCED_FACE ( 'NONE', ( #17132 ), #3810, .F. ) ;
#8940 = CIRCLE ( 'NONE', #12683, 11.50000000000000000 ) ;
#8941 = LINE ( 'NONE', #18695, #10285 ) ;
#8942 = CARTESIAN_POINT ( 'NONE',  ( 2.222972768810839383, -11.17563879758428769, -19.14567149935257007 ) ) ;
#8943 = EDGE_LOOP ( 'NONE', ( #4716, #14205, #7759, #18297, #11121, #11388 ) ) ;
#8944 = CYLINDRICAL_SURFACE ( 'NONE', #15750, 7.500000000000000000 ) ;
#8945 = CARTESIAN_POINT ( 'NONE',  ( 19.99999999999999645, 0.000000000000000000, 0.000000000000000000 ) ) ;
#8946 = EDGE_LOOP ( 'NONE', ( #8056, #12185 ) ) ;
#8947 = AXIS2_PLACEMENT_3D ( 'NONE', #890, #7030, #3947 ) ;
#8948 = DIRECTION ( 'NONE',  ( 0.000000000000000000, 0.000000000000000000, 1.000000000000000000 ) ) ;
#8949 = ORIENTED_EDGE ( 'NONE', *, *, #4275, .T. ) ;
#8950 = CARTESIAN_POINT ( 'NONE',  ( 10.19618095414378800, 15.25966316918061416, -15.86410624981969164 ) ) ;
#8951 = DIRECTION ( 'NONE',  ( 0.000000000000000000, 0.1361666490962466225, -0.9906859460363307557 ) ) ;
#8952 = DIRECTION ( 'NONE',  ( 0.000000000000000000, 0.000000000000000000, -1.000000000000000000 ) ) ;
#8953 = VERTEX_POINT ( 'NONE', #19975 ) ;
#8954 = EDGE_CURVE ( 'NONE', #8604, #20034, #10251, .T. ) ;
#8955 = CYLINDRICAL_SURFACE ( 'NONE', #10236, 65.24900000006525147 ) ;
#8956 = ORIENTED_EDGE ( 'NONE', *, *, #7397, .T. ) ;
#8957 = CIRCLE ( 'NONE', #2533, 65.24900000006525147 ) ;
#8958 = PLANE ( 'NONE',  #20373 ) ;
#8959 = EDGE_CURVE ( 'NONE', #2251, #4710, #11597, .T. ) ;
#8960 = ORIENTED_EDGE ( 'NONE', *, *, #16354, .F. ) ;
#8961 = EDGE_CURVE ( 'NONE', #9123, #12996, #5848, .T. ) ;
#8962 = EDGE_CURVE ( 'NONE', #11972, #4126, #2459, .T. ) ;
#8963 = LINE ( 'NONE', #1021, #7355 ) ;
#8964 = LINE ( 'NONE', #17236, #10592 ) ;
#8965 = CONTEXT_DEPENDENT_SHAPE_REPRESENTATION ( #12811, #15085 ) ;
#8966 = CARTESIAN_POINT ( 'NONE',  ( 8.382925371439633011, 12.54593441562640876, 4.842635668841546170 ) ) ;
#8967 = CLOSED_SHELL ( 'NONE', ( #11767, #11652, #12202, #3741, #17012, #16911, #3006, #2471, #167, #7913, #20811, #1225, #5430, #18574, #18414, #5123, #7509, #13231, #6987, #10841, #16729, #7933, #12476, #18765, #949, #7760, #6605, #3292 ) ) ;
#8968 = ORIENTED_EDGE ( 'NONE', *, *, #17139, .F. ) ;
#8969 = DIRECTION ( 'NONE',  ( 1.000000000000000000, 0.000000000000000000, 0.000000000000000000 ) ) ;
#8970 = ORIENTED_EDGE ( 'NONE', *, *, #20769, .F. ) ;
#8971 = ADVANCED_FACE ( 'NONE', ( #3975 ), #4075, .F. ) ;
#8972 = DIRECTION ( 'NONE',  ( 1.000000000000000000, -0.000000000000000000, -0.000000000000000000 ) ) ;
#8973 = EDGE_CURVE ( 'NONE', #14958, #14416, #4149, .T. ) ;
#8974 = CARTESIAN_POINT ( 'NONE',  ( -2.163827323447877821E-09, -17.99999999999999645, 4.910200000180310553 ) ) ;
#8975 = CARTESIAN_POINT ( 'NONE',  ( 18.00000000000000000, -2.163824016901520184E-09, 23.30855000018031475 ) ) ;
#8976 = AXIS2_PLACEMENT_3D ( 'NONE', #3405, #9126, #12521 ) ;
#8977 = ORIENTED_EDGE ( 'NONE', *, *, #9161, .T. ) ;
#8978 = EDGE_CURVE ( 'NONE', #13237, #4551, #20712, .T. ) ;
#8979 = CARTESIAN_POINT ( 'NONE',  ( 19.99999999999999645, 51.43306257653143376, 40.15061736769582268 ) ) ;
#8980 = FACE_OUTER_BOUND ( 'NONE', #16978, .T. ) ;
#8981 = VERTEX_POINT ( 'NONE', #7899 ) ;
#8982 = CARTESIAN_POINT ( 'NONE',  ( 0.8121682023710344867, -22.99840189857037842, -75.37408292472038340 ) ) ;
#8983 = EDGE_LOOP ( 'NONE', ( #5006, #4825, #5362, #13818 ) ) ;
#8984 = CONICAL_SURFACE ( 'NONE', #5257, 4.000000000000000000, 1.047197551196595855 ) ;
#8985 = CARTESIAN_POINT ( 'NONE',  ( 6.929096493489625530, -2.870125743571142252, 0.9628625001803087224 ) ) ;
#8986 = CARTESIAN_POINT ( 'NONE',  ( 17.99999999999999645, -2.163824016901520184E-09, -16.29604999981969371 ) ) ;
#8987 = VERTEX_POINT ( 'NONE', #9395 ) ;
#8988 = ORIENTED_EDGE ( 'NONE', *, *, #12489, .F. ) ;
#8989 = CARTESIAN_POINT ( 'NONE',  ( 45.93925756638552116, -7.831954179031021646, -85.40612192029891503 ) ) ;
#8990 = DIRECTION ( 'NONE',  ( -1.000000000000000000, -0.000000000000000000, 0.000000000000000000 ) ) ;
#8991 = CYLINDRICAL_SURFACE ( 'NONE', #6477, 27.60000000002760245 ) ;
#8992 = DIRECTION ( 'NONE',  ( 1.000000000000000000, -0.000000000000000000, -0.000000000000000000 ) ) ;
#8993 = CARTESIAN_POINT ( 'NONE',  ( 0.000000000000000000, 0.000000000000000000, 0.000000000000000000 ) ) ;
#8994 = CARTESIAN_POINT ( 'NONE',  ( 3.580422610670021211, -18.00000000043041481, -2.904731249819689776 ) ) ;
#8995 = PRODUCT_DEFINITION_CONTEXT ( 'detailed design', #17546, 'design' ) ;
#8996 = AXIS2_PLACEMENT_3D ( 'NONE', #8427, #15286, #20049 ) ;
#8997 = DIRECTION ( 'NONE',  ( 0.000000000000000000, 0.000000000000000000, -1.000000000000000000 ) ) ;
#8998 = B_SPLINE_CURVE_WITH_KNOTS ( 'NONE', 3,
 ( #15509, #9258, #5861, #12335, #18802, #15720 ),
 .UNSPECIFIED., .F., .F.,
 ( 4, 2, 4 ),
 ( 1.734723475976807094E-18, 0.003996741055817019245, 0.007993482111634036755 ),
 .UNSPECIFIED. ) ;
#8999 = CARTESIAN_POINT ( 'NONE',  ( -6.358192988180021210, -4.248408729364580694, -8.382393749819687656 ) ) ;
#9000 = ORIENTED_EDGE ( 'NONE', *, *, #1952, .F. ) ;
#9001 = CARTESIAN_POINT ( 'NONE',  ( 45.22159793441013420, -8.673994507468389514, -84.62946326583126222 ) ) ;
#9002 = EDGE_CURVE ( 'NONE', #6180, #3647, #17341, .T. ) ;
#9003 = CIRCLE ( 'NONE', #5267, 10.00000000000000178 ) ;
#9004 = CARTESIAN_POINT ( 'NONE',  ( -6.330490858644137298, -9.474249097082495297, -15.66526600028680782 ) ) ;
#9005 = PRODUCT_DEFINITION_SHAPE ( 'NONE', 'NONE',  #20959 ) ;
#9006 = CARTESIAN_POINT ( 'NONE',  ( 19.99999999999999645, -63.17103598352137794, 16.33561182745118501 ) ) ;
#9007 = ORIENTED_EDGE ( 'NONE', *, *, #14780, .F. ) ;
#9008 = CARTESIAN_POINT ( 'NONE',  ( 2.500000000000000000, 1.178949249685212974, -2.042000000000001148 ) ) ;
#9009 = CARTESIAN_POINT ( 'NONE',  ( -16.62983158603122291, -6.888301780572501087, -0.8430124998196862895 ) ) ;
#9010 = CARTESIAN_POINT ( 'NONE',  ( 9.999999999999998224, 70.29359119158485214, 15.58239511117312226 ) ) ;
#9011 = ORIENTED_EDGE ( 'NONE', *, *, #20584, .T. ) ;
#9012 = DIRECTION ( 'NONE',  ( 0.000000000000000000, 0.000000000000000000, -1.000000000000000000 ) ) ;
#9013 = ORIENTED_EDGE ( 'NONE', *, *, #17358, .F. ) ;
#9014 = DIRECTION ( 'NONE',  ( -0.000000000000000000, -0.000000000000000000, -1.000000000000000000 ) ) ;
#9015 = CARTESIAN_POINT ( 'NONE',  ( 0.000000000000000000, -5.762283366690708952, -64.99406197038678101 ) ) ;
#9016 = AXIS2_PLACEMENT_3D ( 'NONE', #13896, #7312, #12097 ) ;
#9017 = VERTEX_POINT ( 'NONE', #9489 ) ;
#9019 = EDGE_LOOP ( 'NONE', ( #9158, #2755, #4344, #19574 ) ) ;
#9018 = B_SPLINE_CURVE_WITH_KNOTS ( 'NONE', 3,
 ( #6252, #4979, #14932, #6861, #16115, #408, #6664, #6450 ),
 .UNSPECIFIED., .F., .F.,
 ( 4, 2, 2, 4 ),
 ( 1.734723475976807094E-18, 0.005430084938242705703, 0.008145127407364069830, 0.01086016987648543569 ),
 .UNSPECIFIED. ) ;
#9020 = CARTESIAN_POINT ( 'NONE',  ( 19.99999999999999645, -68.15657073222419626, -23.20952102120349991 ) ) ;
#9021 = VECTOR ( 'NONE', #16379, 1000.000000000000000 ) ;
#9022 = CIRCLE ( 'NONE', #2250, 27.60000000002759535 ) ;
#9023 = EDGE_CURVE ( 'NONE', #7461, #8404, #786, .T. ) ;
#9024 = FACE_OUTER_BOUND ( 'NONE', #3111, .T. ) ;
#9025 = AXIS2_PLACEMENT_3D ( 'NONE', #13793, #20243, #18240 ) ;
#9026 = CARTESIAN_POINT ( 'NONE',  ( 150.0000507999999968, 4.898587196589412829E-16, -4.000000000000000000 ) ) ;
#9027 = CIRCLE ( 'NONE', #2607, 2.649999999999999467 ) ;
#9028 = CARTESIAN_POINT ( 'NONE',  ( -7.500000000000000888, 9.015942588607330751E-10, -4.338699999819690234 ) ) ;
#9029 = AXIS2_PLACEMENT_3D ( 'NONE', #14428, #1299, #9124 ) ;
#9030 = DIRECTION ( 'NONE',  ( 0.000000000000000000, -1.000000000000000000, 0.000000000000000000 ) ) ;
#9031 = CARTESIAN_POINT ( 'NONE',  ( 19.99999999999999645, -35.35772184876843482, -54.34979580218228534 ) ) ;
#9032 = CARTESIAN_POINT ( 'NONE',  ( 19.99999999999999645, 11.98658579560678206, -64.13855129306456604 ) ) ;
#9033 = DIRECTION ( 'NONE',  ( 1.000000000000000000, 0.000000000000000000, 0.000000000000000000 ) ) ;
#9034 = AXIS2_PLACEMENT_3D ( 'NONE', #18157, #3328, #461 ) ;
#9035 = ORIENTED_EDGE ( 'NONE', *, *, #14468, .F. ) ;
#9036 = CYLINDRICAL_SURFACE ( 'NONE', #2768, 72.00000000007199219 ) ;
#9037 = EDGE_LOOP ( 'NONE', ( #5344, #168, #14809, #4094 ) ) ;
#9038 = CARTESIAN_POINT ( 'NONE',  ( -18.00000000000000000, 2.163826221265758884E-09, 7.266450000180315172 ) ) ;
#9039 = CARTESIAN_POINT ( 'NONE',  ( 9.999999999999998224, -58.26603306961992956, 42.29739224042451440 ) ) ;
#9040 = ORIENTED_EDGE ( 'NONE', *, *, #3026, .T. ) ;
#9041 = CARTESIAN_POINT ( 'NONE',  ( 0.000000000000000000, -39.37110852956848817, 51.51683813304857296 ) ) ;
#9042 = ORIENTED_EDGE ( 'NONE', *, *, #10981, .T. ) ;
#9043 = EDGE_CURVE ( 'NONE', #6265, #10714, #3478, .T. ) ;
#9044 = DIRECTION ( 'NONE',  ( 0.000000000000000000, 0.000000000000000000, 1.000000000000000000 ) ) ;
#9045 = CARTESIAN_POINT ( 'NONE',  ( 2.500000000000000000, 0.000000000000000000, 0.000000000000000000 ) ) ;
#9046 = AXIS2_PLACEMENT_3D ( 'NONE', #7616, #11335, #16923 ) ;
#9047 = ORIENTED_EDGE ( 'NONE', *, *, #10403, .T. ) ;
#9048 = DIRECTION ( 'NONE',  ( -1.000000000000000000, 0.000000000000000000, -0.000000000000000000 ) ) ;
#9049 = ADVANCED_FACE ( 'NONE', ( #14381 ), #11090, .T. ) ;
#9050 = VECTOR ( 'NONE', #7049, 1000.000000000000000 ) ;
#9051 = CARTESIAN_POINT ( 'NONE',  ( 2.000000000000010658, -3.464101615137748169, 0.000000000000000000 ) ) ;
#9052 = FACE_OUTER_BOUND ( 'NONE', #15495, .T. ) ;
#9053 = CARTESIAN_POINT ( 'NONE',  ( 1.040949779275250179E-14, -85.00000000000000000, 19.00000000000000000 ) ) ;
#9054 = AXIS2_PLACEMENT_3D ( 'NONE', #9810, #3143, #5039 ) ;
#9055 = AXIS2_PLACEMENT_3D ( 'NONE', #8463, #5390, #2118 ) ;
#9056 = DIRECTION ( 'NONE',  ( -0.000000000000000000, -0.000000000000000000, 1.000000000000000000 ) ) ;
#9057 = EDGE_CURVE ( 'NONE', #7334, #6474, #10938, .T. ) ;
#9058 = ORIENTED_EDGE ( 'NONE', *, *, #26, .T. ) ;
#9059 =( NAMED_UNIT ( * ) SI_UNIT ( $, .STERADIAN. ) SOLID_ANGLE_UNIT ( ) );
#9060 = CARTESIAN_POINT ( 'NONE',  ( 0.000000000000000000, -1.178949249685218748, -2.041999999999998039 ) ) ;
#9061 = ORIENTED_EDGE ( 'NONE', *, *, #18922, .F. ) ;
#9062 = AXIS2_PLACEMENT_3D ( 'NONE', #20727, #19748, #16081 ) ;
#9063 = CARTESIAN_POINT ( 'NONE',  ( -1.588862400715383316, -21.45483734977869261, -70.59898835680725426 ) ) ;
#9064 = DIRECTION ( 'NONE',  ( -0.000000000000000000, -0.000000000000000000, 1.000000000000000000 ) ) ;
#9065 = ORIENTED_EDGE ( 'NONE', *, *, #13558, .T. ) ;
#9066 = CIRCLE ( 'NONE', #20905, 65.24900000006525147 ) ;
#9067 = CARTESIAN_POINT ( 'NONE',  ( -3.580422610670018546, 18.00000000043041126, -17.04223124981968596 ) ) ;
#9068 = CARTESIAN_POINT ( 'NONE',  ( -30.00000000000000000, 29.99999999999999289, -120.0000000000000142 ) ) ;
#9069 = DIRECTION ( 'NONE',  ( -0.000000000000000000, -0.000000000000000000, 1.000000000000000000 ) ) ;
#9070 = ORIENTED_EDGE ( 'NONE', *, *, #8907, .T. ) ;
#9071 = AXIS2_PLACEMENT_3D ( 'NONE', #20588, #12537, #17622 ) ;
#9072 = DIRECTION ( 'NONE',  ( -1.000000000000000000, -0.000000000000000000, -0.000000000000000000 ) ) ;
#9073 = ORIENTED_EDGE ( 'NONE', *, *, #20247, .T. ) ;
#9074 = CARTESIAN_POINT ( 'NONE',  ( 7.500000000000008882, 1.491842754878802690, 15.76916875008778973 ) ) ;
#9075 = EDGE_LOOP ( 'NONE', ( #9359, #6431, #7739, #19746 ) ) ;
#9076 = FACE_OUTER_BOUND ( 'NONE', #4020, .T. ) ;
#9077 = DIRECTION ( 'NONE',  ( -1.000000000000000000, -0.000000000000000000, -0.000000000000000000 ) ) ;
#9078 = SHAPE_DEFINITION_REPRESENTATION ( #3557, #4392 ) ;
#9079 = CARTESIAN_POINT ( 'NONE',  ( 8.382925368423272516, -12.54593441764187745, 7.787948168841544394 ) ) ;
#9080 = EDGE_CURVE ( 'NONE', #5761, #7195, #11184, .T. ) ;
#9081 = ORIENTED_EDGE ( 'NONE', *, *, #18173, .F. ) ;
#9082 = EDGE_CURVE ( 'NONE', #17178, #16888, #10870, .T. ) ;
#9083 = CARTESIAN_POINT ( 'NONE',  ( 0.000000000000000000, -2.357898499370432166, 3.035766082959412415E-15 ) ) ;
#9084 = EDGE_LOOP ( 'NONE', ( #11175, #15097, #11446, #12618 ) ) ;
#9085 = DIRECTION ( 'NONE',  ( 0.000000000000000000, 3.469446951953615175E-16, 1.000000000000000000 ) ) ;
#9086 = CARTESIAN_POINT ( 'NONE',  ( -3.580422610670017658, 18.00000000043040771, 9.328168750180312330 ) ) ;
#9087 = LINE ( 'NONE', #15538, #6137 ) ;
#9088 = DIRECTION ( 'NONE',  ( 1.000000000000000000, -0.000000000000000000, -0.000000000000000000 ) ) ;
#9089 = ADVANCED_FACE ( 'NONE', ( #14174 ), #2816, .T. ) ;
#9090 = ORIENTED_EDGE ( 'NONE', *, *, #9606, .F. ) ;
#9091 = CARTESIAN_POINT ( 'NONE',  ( 19.99999999999999645, -64.79224928664389438, -2.456263514198281150 ) ) ;
#9092 = LINE ( 'NONE', #17036, #7018 ) ;
#9093 = ORIENTED_EDGE ( 'NONE', *, *, #11345, .F. ) ;
#9094 = DIRECTION ( 'NONE',  ( 1.000000000000000000, -0.000000000000000000, -0.000000000000000000 ) ) ;
#9095 = CARTESIAN_POINT ( 'NONE',  ( 19.99999999999999645, -60.35829202194859278, -24.78524934717612282 ) ) ;
#9096 = CARTESIAN_POINT ( 'NONE',  ( 3.580422610670019878, -18.00000000043040771, -14.23433124981968945 ) ) ;
#9097 = ORIENTED_EDGE ( 'NONE', *, *, #8710, .F. ) ;
#9098 = ORIENTED_EDGE ( 'NONE', *, *, #2612, .F. ) ;
#9099 = CARTESIAN_POINT ( 'NONE',  ( 19.99999999999999645, -28.84646472442415543, -58.52617768068463278 ) ) ;
#9100 = EDGE_CURVE ( 'NONE', #3970, #11744, #4821, .T. ) ;
#9101 = DIRECTION ( 'NONE',  ( 1.000000000000000000, -0.000000000000000000, -0.000000000000000000 ) ) ;
#9102 = CARTESIAN_POINT ( 'NONE',  ( 0.000000000000000000, 0.000000000000000000, 40.00000000000000000 ) ) ;
#9103 = CARTESIAN_POINT ( 'NONE',  ( -52.49999999999999289, -130.0000000000000000, 5.000000000000000000 ) ) ;
#9104 = CARTESIAN_POINT ( 'NONE',  ( -16.62983158603122646, -6.888301780572501976, -0.8430124998196897312 ) ) ;
#9105 = ADVANCED_FACE ( 'NONE', ( #9176 ), #15634, .T. ) ;
#9106 = EDGE_CURVE ( 'NONE', #19457, #13026, #1135, .T. ) ;
#9107 = PLANE ( 'NONE',  #6549 ) ;
#9108 = ORIENTED_EDGE ( 'NONE', *, *, #15798, .T. ) ;
#9109 = CARTESIAN_POINT ( 'NONE',  ( 24.99999999999999645, -39.99999999999999289, -54.09999999999999432 ) ) ;
#9110 = CARTESIAN_POINT ( 'NONE',  ( 5.663308646854338768, -13.67243654778934747, 11.88939558151907683 ) ) ;
#9111 = EDGE_CURVE ( 'NONE', #3661, #20364, #117, .T. ) ;
#9112 = DIRECTION ( 'NONE',  ( 0.000000000000000000, -0.000000000000000000, -1.000000000000000000 ) ) ;
#9113 = ORIENTED_EDGE ( 'NONE', *, *, #12362, .F. ) ;
#9114 = CARTESIAN_POINT ( 'NONE',  ( -9.850000000000006750, 0.000000000000000000, 43.00000000000000000 ) ) ;
#9115 = DIRECTION ( 'NONE',  ( 1.000000000000000000, 0.000000000000000000, 0.000000000000000000 ) ) ;
#9116 = DIRECTION ( 'NONE',  ( -1.000000000000000000, 0.000000000000000000, -0.000000000000000000 ) ) ;
#9117 = ORIENTED_EDGE ( 'NONE', *, *, #11676, .T. ) ;
#9118 = DIRECTION ( 'NONE',  ( -1.000000000000000000, -0.000000000000000000, -0.000000000000000000 ) ) ;
#9119 = ORIENTED_EDGE ( 'NONE', *, *, #11699, .T. ) ;
#9120 = DIRECTION ( 'NONE',  ( 1.000000000000000000, 1.836909530733573776E-16, 0.000000000000000000 ) ) ;
#9121 = DIRECTION ( 'NONE',  ( -1.000000000000000000, -0.000000000000000000, 0.000000000000000000 ) ) ;
#9122 = ORIENTED_EDGE ( 'NONE', *, *, #5809, .T. ) ;
#9123 = VERTEX_POINT ( 'NONE', #20516 ) ;
#9124 = DIRECTION ( 'NONE',  ( 0.000000000000000000, 0.000000000000000000, 1.000000000000000000 ) ) ;
#9125 = ADVANCED_FACE ( 'NONE', ( #5997 ), #19734, .T. ) ;
#9126 = DIRECTION ( 'NONE',  ( 0.000000000000000000, 0.000000000000000000, 1.000000000000000000 ) ) ;
#9127 = FACE_OUTER_BOUND ( 'NONE', #10253, .T. ) ;
#9128 = ADVANCED_FACE ( 'NONE', ( #6091 ), #3160, .F. ) ;
#9129 = LINE ( 'NONE', #14330, #12928 ) ;
#9130 = CARTESIAN_POINT ( 'NONE',  ( -7.499999999820661678, 1.491842756249031288, -22.89416874981969130 ) ) ;
#9131 = CARTESIAN_POINT ( 'NONE',  ( 19.99999999999999645, 0.000000000000000000, 0.000000000000000000 ) ) ;
#9132 = DIRECTION ( 'NONE',  ( -0.000000000000000000, -0.000000000000000000, 1.000000000000000000 ) ) ;
#9133 = CARTESIAN_POINT ( 'NONE',  ( 0.000000000000000000, -5.762283366691622000, 64.99406197038668154 ) ) ;
#9134 = ORIENTED_EDGE ( 'NONE', *, *, #18959, .T. ) ;
#9135 = EDGE_CURVE ( 'NONE', #20910, #12110, #9263, .T. ) ;
#9136 = FACE_OUTER_BOUND ( 'NONE', #7475, .T. ) ;
#9137 = ORIENTED_EDGE ( 'NONE', *, *, #14530, .F. ) ;
#9138 = CARTESIAN_POINT ( 'NONE',  ( 10.19618095414378800, 15.25966316918061416, -8.343706249819687670 ) ) ;
#9139 = CARTESIAN_POINT ( 'NONE',  ( 19.99999999999999645, 0.000000000000000000, 0.000000000000000000 ) ) ;
#9140 =( REPRESENTATION_RELATIONSHIP ('NONE','NONE', #13739, #20346 ) REPRESENTATION_RELATIONSHIP_WITH_TRANSFORMATION ( #7151 )SHAPE_REPRESENTATION_RELATIONSHIP( ) );
#9141 = EDGE_LOOP ( 'NONE', ( #14870, #2222, #1045, #9580 ) ) ;
#9142 = DIRECTION ( 'NONE',  ( 1.000000000000000000, 0.000000000000000000, 0.000000000000000000 ) ) ;
#9143 = ORIENTED_EDGE ( 'NONE', *, *, #2506, .T. ) ;
#9144 = FACE_OUTER_BOUND ( 'NONE', #19169, .T. ) ;
#9145 = DIRECTION ( 'NONE',  ( 1.000000000000000000, 0.000000000000000000, 0.000000000000000000 ) ) ;
#9146 = DIRECTION ( 'NONE',  ( -1.000000000000000000, 0.000000000000000000, 0.000000000000000000 ) ) ;
#9147 = EDGE_LOOP ( 'NONE', ( #13185, #3574, #18650, #458 ) ) ;
#9148 = CARTESIAN_POINT ( 'NONE',  ( 6.929096493489630859, -2.870125743571144472, -21.04723749981969050 ) ) ;
#9149 = DIRECTION ( 'NONE',  ( 1.000000000000000000, 0.000000000000000000, 0.000000000000000000 ) ) ;
#9150 = CARTESIAN_POINT ( 'NONE',  ( -3.580422610670017658, 18.00000000043040771, -18.94683124981969158 ) ) ;
#9151 = CARTESIAN_POINT ( 'NONE',  ( 19.99999999999999645, 10.77748419466696284, 63.93680186330476545 ) ) ;
#9152 = VECTOR ( 'NONE', #3216, 1000.000000000000000 ) ;
#9153 = CARTESIAN_POINT ( 'NONE',  ( 0.000000000000000000, -38.22257254261699444, -61.01667762370178139 ) ) ;
#9154 = VERTEX_POINT ( 'NONE', #16170 ) ;
#9155 = SURFACE_SIDE_STYLE ('',( #10758 ) ) ;
#9156 = CARTESIAN_POINT ( 'NONE',  ( -12.50000000000000533, 0.000000000000000000, 43.00000000000000000 ) ) ;
#9157 = AXIS2_PLACEMENT_3D ( 'NONE', #2034, #6903, #17084 ) ;
#9158 = ORIENTED_EDGE ( 'NONE', *, *, #10133, .T. ) ;
#9159 = DIRECTION ( 'NONE',  ( 0.000000000000000000, 0.000000000000000000, 1.000000000000000000 ) ) ;
#9160 = FACE_OUTER_BOUND ( 'NONE', #7379, .T. ) ;
#9161 = EDGE_CURVE ( 'NONE', #10032, #14416, #16567, .T. ) ;
#9162 = EDGE_LOOP ( 'NONE', ( #2713, #12816 ) ) ;
#9163 = EDGE_CURVE ( 'NONE', #9439, #5992, #2481, .T. ) ;
#9164 = CARTESIAN_POINT ( 'NONE',  ( 15.25966316918061416, -10.19618095414378622, -13.50785624981968702 ) ) ;
#9165 = CYLINDRICAL_SURFACE ( 'NONE', #15778, 65.24900000006525147 ) ;
#9166 = CARTESIAN_POINT ( 'NONE',  ( 0.000000000000000000, 45.48683723007275148, -46.78012013466171481 ) ) ;
#9167 = ORIENTED_EDGE ( 'NONE', *, *, #9338, .T. ) ;
#9168 = DIRECTION ( 'NONE',  ( -0.1159034202170323435, 1.393303357259113989E-11, -0.9932604880805406822 ) ) ;
#9169 = ORIENTED_EDGE ( 'NONE', *, *, #1882, .F. ) ;
#9170 = CARTESIAN_POINT ( 'NONE',  ( 9.999999999999998224, -18.50424539729797146, -69.58155576219135696 ) ) ;
#9171 = CIRCLE ( 'NONE', #7121, 8.999999999999994671 ) ;
#9172 = EDGE_LOOP ( 'NONE', ( #5547, #830 ) ) ;
#9173 = VECTOR ( 'NONE', #9447, 1000.000000000000000 ) ;
#9174 = CIRCLE ( 'NONE', #11871, 17.50000000000000355 ) ;
#9175 = LINE ( 'NONE', #7467, #14494 ) ;
#9176 = FACE_OUTER_BOUND ( 'NONE', #16019, .T. ) ;
#9177 = CARTESIAN_POINT ( 'NONE',  ( -13.67243654642775574, 5.663308650141533285, -7.233145581158455961 ) ) ;
#9178 = ORIENTED_EDGE ( 'NONE', *, *, #5598, .F. ) ;
#9179 = FACE_OUTER_BOUND ( 'NONE', #16798, .T. ) ;
#9180 = ORIENTED_EDGE ( 'NONE', *, *, #14275, .T. ) ;
#9181 = CARTESIAN_POINT ( 'NONE',  ( 14.14403058282573689, -16.24569260159238837, 78.86174789526529594 ) ) ;
#9182 = CIRCLE ( 'NONE', #7835, 4.000000000000000000 ) ;
#9183 = CARTESIAN_POINT ( 'NONE',  ( 10.19618095414378622, 15.25966316918061239, 1.081293750180310820 ) ) ;
#9184 = LINE ( 'NONE', #7912, #16964 ) ;
#9185 = CIRCLE ( 'NONE', #13582, 65.24900000006525147 ) ;
#9186 = CARTESIAN_POINT ( 'NONE',  ( 19.99999999999999645, -5.762283366690708064, -64.99406197038676680 ) ) ;
#9187 = ORIENTED_EDGE ( 'NONE', *, *, #1614, .T. ) ;
#9188 = CYLINDRICAL_SURFACE ( 'NONE', #17164, 27.60000000002759890 ) ;
#9189 = DIRECTION ( 'NONE',  ( 1.000000000000000000, -0.000000000000000000, -0.000000000000000000 ) ) ;
#9190 = COLOUR_RGB ( '', 0.66274510, 0.83137255, 0.94901961) ;
#9191 = VERTEX_POINT ( 'NONE', #11595 ) ;
#9192 = EDGE_CURVE ( 'NONE', #19322, #17178, #1805, .T. ) ;
#9193 = CARTESIAN_POINT ( 'NONE',  ( 20.21512691275406937, -10.97478183557446307, -82.63187968860285082 ) ) ;
#9194 = LINE ( 'NONE', #7385, #1425 ) ;
#9195 = CARTESIAN_POINT ( 'NONE',  ( -17.99999999956958163, 3.580422614997673669, -11.28901874981968945 ) ) ;
#9196 = VERTEX_POINT ( 'NONE', #3336 ) ;
#9197 = AXIS2_PLACEMENT_3D ( 'NONE', #9200, #12495, #12387 ) ;
#9198 = AXIS2_PLACEMENT_3D ( 'NONE', #10831, #12321, #2455 ) ;
#9199 = LINE ( 'NONE', #2840, #2778 ) ;
#9200 = CARTESIAN_POINT ( 'NONE',  ( 0.000000000000000000, 0.000000000000000000, 0.000000000000000000 ) ) ;
#9201 = LINE ( 'NONE', #12167, #13285 ) ;
#9202 = AXIS2_PLACEMENT_3D ( 'NONE', #9836, #1893, #11638 ) ;
#9203 = EDGE_CURVE ( 'NONE', #2027, #3467, #17727, .T. ) ;
#9204 = DIRECTION ( 'NONE',  ( 1.224646799147353207E-16, -4.064521778635712183E-50, -1.000000000000000000 ) ) ;
#9205 = CARTESIAN_POINT ( 'NONE',  ( 12.72792206288791128, 12.72792205982780267, 3.280425000180310580 ) ) ;
#9206 = EDGE_CURVE ( 'NONE', #9763, #5350, #9702, .T. ) ;
#9207 = DIRECTION ( 'NONE',  ( 1.000000000000000000, 0.000000000000000000, 0.000000000000000000 ) ) ;
#9208 = ORIENTED_EDGE ( 'NONE', *, *, #19207, .F. ) ;
#9209 = STYLED_ITEM ( 'NONE', ( #4848 ), #17543 ) ;
#9210 = CARTESIAN_POINT ( 'NONE',  ( -7.500000000000007994, -1.491842754878805355, 20.48166875008779542 ) ) ;
#9211 = CARTESIAN_POINT ( 'NONE',  ( -13.67243654778935102, -5.663308646854334327, 4.820645581519075407 ) ) ;
#9212 = CARTESIAN_POINT ( 'NONE',  ( 1.040949779275250179E-14, -85.00000000000000000, 19.00000000000000000 ) ) ;
#9213 = ORIENTED_EDGE ( 'NONE', *, *, #17105, .T. ) ;
#9214 = CARTESIAN_POINT ( 'NONE',  ( -31.35784117651625635, 26.35784117651607872, -120.0000000000000142 ) ) ;
#9215 = CARTESIAN_POINT ( 'NONE',  ( -2.163827323447878234E-09, -18.00000000000000000, -21.46019999981968951 ) ) ;
#9216 = DIRECTION ( 'NONE',  ( 1.000000000000000000, 0.000000000000000000, 0.000000000000000000 ) ) ;
#9217 = AXIS2_PLACEMENT_3D ( 'NONE', #7087, #325, #10080 ) ;
#9218 = ORIENTED_EDGE ( 'NONE', *, *, #4688, .T. ) ;
#9219 = EDGE_CURVE ( 'NONE', #15337, #3206, #20056, .T. ) ;
#9220 = DIRECTION ( 'NONE',  ( 0.000000000000000000, 0.000000000000000000, -1.000000000000000000 ) ) ;
#9221 = VERTEX_POINT ( 'NONE', #19861 ) ;
#9222 = CARTESIAN_POINT ( 'NONE',  ( 0.000000000000000000, 0.000000000000000000, -90.00000000000000000 ) ) ;
#9223 = CARTESIAN_POINT ( 'NONE',  ( 0.000000000000000000, -36.54710069451090959, 54.05313526368099986 ) ) ;
#9224 = EDGE_CURVE ( 'NONE', #15415, #5413, #8309, .T. ) ;
#9225 = EDGE_LOOP ( 'NONE', ( #10634, #1342, #2071, #10842 ) ) ;
#9226 = EDGE_LOOP ( 'NONE', ( #7387, #2372, #20863, #18884 ) ) ;
#9227 = CARTESIAN_POINT ( 'NONE',  ( 33.68763977253520636, -116.6032510994795217, -76.49582849428456655 ) ) ;
#9228 = EDGE_CURVE ( 'NONE', #18900, #2782, #13644, .T. ) ;
#9229 =( NAMED_UNIT ( * ) SI_UNIT ( $, .STERADIAN. ) SOLID_ANGLE_UNIT ( ) );
#9230 = CARTESIAN_POINT ( 'NONE',  ( 9.470358143689582064, -1.138454911109690799E-09, 8.603271702811174038 ) ) ;
#9231 = CIRCLE ( 'NONE', #13300, 4.250000000000000000 ) ;
#9232 = CARTESIAN_POINT ( 'NONE',  ( 3.999999999999990674, -2.309401076758548221, -0.3572655899081733644 ) ) ;
#9233 = AXIS2_PLACEMENT_3D ( 'NONE', #3147, #9812, #7717 ) ;
#9234 = CARTESIAN_POINT ( 'NONE',  ( 7.500000000179339210, 1.491842754445841690, -18.77073124981968988 ) ) ;
#9235 = LINE ( 'NONE', #12313, #13933 ) ;
#9236 = CIRCLE ( 'NONE', #99, 27.60000000002759890 ) ;
#9237 = EDGE_CURVE ( 'NONE', #13848, #4671, #4924, .T. ) ;
#9238 = PLANE ( 'NONE',  #16140 ) ;
#9239 = DIRECTION ( 'NONE',  ( -0.000000000000000000, -0.000000000000000000, 1.000000000000000000 ) ) ;
#9240 = EDGE_CURVE ( 'NONE', #12110, #12459, #8204, .T. ) ;
#9241 = VERTEX_POINT ( 'NONE', #16475 ) ;
#9242 = CARTESIAN_POINT ( 'NONE',  ( 9.999999999999998224, -71.76067541710854414, 5.865617076724380041 ) ) ;
#9243 = ORIENTED_EDGE ( 'NONE', *, *, #12362, .T. ) ;
#9244 = CARTESIAN_POINT ( 'NONE',  ( -16.62983158437510056, 6.888301784570729502, -10.99448749981968554 ) ) ;
#9245 = LINE ( 'NONE', #1095, #7595 ) ;
#9246 = CIRCLE ( 'NONE', #12972, 4.000000000000000888 ) ;
#9247 = ORIENTED_EDGE ( 'NONE', *, *, #11428, .F. ) ;
#9248 = CIRCLE ( 'NONE', #10270, 7.500000000000000888 ) ;
#9249 = CARTESIAN_POINT ( 'NONE',  ( 19.99999999999999645, -10.74906464462167577, 71.19310085447963843 ) ) ;
#9250 = VERTEX_POINT ( 'NONE', #6812 ) ;
#9251 = CARTESIAN_POINT ( 'NONE',  ( -4.000000000000000000, -2.309401076758525573, -5.599999999999999645 ) ) ;
#9252 = CARTESIAN_POINT ( 'NONE',  ( 30.43430782549247837, -42.57363661491096707, -71.38288848018790134 ) ) ;
#9253 = DIRECTION ( 'NONE',  ( 0.000000000000000000, 0.000000000000000000, 1.000000000000000000 ) ) ;
#9254 = EDGE_CURVE ( 'NONE', #16423, #16359, #19070, .T. ) ;
#9255 = VERTEX_POINT ( 'NONE', #8109 ) ;
#9256 = FACE_BOUND ( 'NONE', #7919, .T. ) ;
#9257 = CIRCLE ( 'NONE', #4851, 27.60000000002759890 ) ;
#9258 = CARTESIAN_POINT ( 'NONE',  ( 45.93925756638542879, -7.831954179031023422, 85.40612192029894345 ) ) ;
#9259 = LINE ( 'NONE', #13925, #4593 ) ;
#9260 = LINE ( 'NONE', #20688, #14383 ) ;
#9261 = AXIS2_PLACEMENT_3D ( 'NONE', #9230, #16007, #12415 ) ;
#9262 = CYLINDRICAL_SURFACE ( 'NONE', #17408, 2.649999999999999467 ) ;
#9263 = CIRCLE ( 'NONE', #18733, 27.60000000002760245 ) ;
#9265 = EDGE_LOOP ( 'NONE', ( #13342, #1945 ) ) ;
#9264 = AXIS2_PLACEMENT_3D ( 'NONE', #14550, #224, #3396 ) ;
#9266 = CARTESIAN_POINT ( 'NONE',  ( 6.165579999999999394, 1.321856812770071588E-15, -10.79377999999999993 ) ) ;
#9267 = DIRECTION ( 'NONE',  ( -1.000000000000000000, -0.000000000000000000, -0.000000000000000000 ) ) ;
#9268 = ORIENTED_EDGE ( 'NONE', *, *, #19593, .T. ) ;
#9269 = CARTESIAN_POINT ( 'NONE',  ( 23.13963350654227824, -26.35784117651622793, -120.0000000000000142 ) ) ;
#9270 = CARTESIAN_POINT ( 'NONE',  ( 0.000000000000000000, 67.51707036274449081, -25.00890260772307627 ) ) ;
#9271 = VERTEX_POINT ( 'NONE', #14580 ) ;
#9272 = CARTESIAN_POINT ( 'NONE',  ( 18.00000000043041126, 3.580422610670019434, -5.260981249819686845 ) ) ;
#9273 = DIRECTION ( 'NONE',  ( 0.000000000000000000, 0.000000000000000000, 1.000000000000000000 ) ) ;
#9274 = DIRECTION ( 'NONE',  ( -1.000000000000000000, 0.000000000000000000, -0.000000000000000000 ) ) ;
#9275 = AXIS2_PLACEMENT_3D ( 'NONE', #18151, #5516, #10510 ) ;
#9276 = VERTEX_POINT ( 'NONE', #13297 ) ;
#9277 = CIRCLE ( 'NONE', #3505, 75.00000000000000000 ) ;
#9278 = CARTESIAN_POINT ( 'NONE',  ( 0.000000000000000000, 0.000000000000000000, 166.0000000000000000 ) ) ;
#9279 = ORIENTED_EDGE ( 'NONE', *, *, #15416, .T. ) ;
#9280 = DIRECTION ( 'NONE',  ( 0.000000000000000000, 0.000000000000000000, -1.000000000000000000 ) ) ;
#9281 = EDGE_LOOP ( 'NONE', ( #13992, #10630, #10058, #8104 ) ) ;
#9282 = AXIS2_PLACEMENT_3D ( 'NONE', #18914, #1535, #17432 ) ;
#9283 = CIRCLE ( 'NONE', #2518, 27.60000000002759890 ) ;
#9284 = CARTESIAN_POINT ( 'NONE',  ( 30.98133542675971341, -111.2038170487246447, 74.06521627071094827 ) ) ;
#9285 = EDGE_CURVE ( 'NONE', #4186, #4931, #12304, .T. ) ;
#9286 = DIRECTION ( 'NONE',  ( -1.000000000000000000, 0.000000000000000000, -0.000000000000000000 ) ) ;
#9287 = CARTESIAN_POINT ( 'NONE',  ( 5.663308650141532397, 13.67243654642775574, -4.876895581158458448 ) ) ;
#9288 = VERTEX_POINT ( 'NONE', #6608 ) ;
#9289 = CARTESIAN_POINT ( 'NONE',  ( 19.99999999999999645, -64.44931368725514176, -10.18420179740675380 ) ) ;
#9290 = EDGE_LOOP ( 'NONE', ( #10881, #817 ) ) ;
#9291 = AXIS2_PLACEMENT_3D ( 'NONE', #8291, #19532, #19625 ) ;
#9292 = CARTESIAN_POINT ( 'NONE',  ( -7.500000000000004441, -1.491842754878798916, -23.48323124991221178 ) ) ;
#9293 = CARTESIAN_POINT ( 'NONE',  ( -12.72792206288790950, -12.72792205982779556, 6.088325000180311086 ) ) ;
#9294 = AXIS2_PLACEMENT_3D ( 'NONE', #18334, #19917, #5395 ) ;
#9295 = CARTESIAN_POINT ( 'NONE',  ( 5.303300859536631329, 5.303300858261585482, -19.65432499981969627 ) ) ;
#9296 = DIRECTION ( 'NONE',  ( 0.000000000000000000, 0.000000000000000000, 1.000000000000000000 ) ) ;
#9297 = VERTEX_POINT ( 'NONE', #10114 ) ;
#9298 = DIRECTION ( 'NONE',  ( 0.000000000000000000, 0.000000000000000000, 1.000000000000000000 ) ) ;
#9299 = DIRECTION ( 'NONE',  ( -1.000000000000000000, 0.000000000000000000, 0.000000000000000000 ) ) ;
#9300 = ORIENTED_EDGE ( 'NONE', *, *, #18528, .T. ) ;
#9301 = CARTESIAN_POINT ( 'NONE',  ( 9.663423836078200324, -20.87488706538416139, -76.33627221503081728 ) ) ;
#9302 = DIRECTION ( 'NONE',  ( 1.000000000000000000, 0.000000000000000000, 0.000000000000000000 ) ) ;
#9303 = CARTESIAN_POINT ( 'NONE',  ( 17.99999999956957808, -3.580422614997675446, -16.00151874981969158 ) ) ;
#9304 = ORIENTED_EDGE ( 'NONE', *, *, #16442, .F. ) ;
#9305 = CARTESIAN_POINT ( 'NONE',  ( 52.50000000000000000, -120.0000000000000142, 0.000000000000000000 ) ) ;
#9306 = FACE_OUTER_BOUND ( 'NONE', #15945, .T. ) ;
#9307 = EDGE_CURVE ( 'NONE', #3802, #6246, #19548, .T. ) ;
#9308 = PLANE ( 'NONE',  #17683 ) ;
#9309 = CARTESIAN_POINT ( 'NONE',  ( -12.50000000000000533, 0.000000000000000000, -43.00000000000000000 ) ) ;
#9310 = DIRECTION ( 'NONE',  ( 1.000000000000000000, 0.000000000000000000, 0.000000000000000000 ) ) ;
#9311 = CARTESIAN_POINT ( 'NONE',  ( -18.00000000043041481, -3.580422610670022987, -0.5484812498196925956 ) ) ;
#9312 = CARTESIAN_POINT ( 'NONE',  ( -5.303300859536636658, -5.303300858261589035, -18.10192499981969050 ) ) ;
#9313 = VERTEX_POINT ( 'NONE', #2053 ) ;
#9314 = PRODUCT_DEFINITION_FORMATION_WITH_SPECIFIED_SOURCE ( 'ANY', '', #3902, .NOT_KNOWN. ) ;
#9315 = DIRECTION ( 'NONE',  ( -1.000000000000000000, 0.000000000000000000, 0.000000000000000000 ) ) ;
#9316 = ADVANCED_FACE ( 'NONE', ( #1958 ), #14990, .T. ) ;
#9317 = CARTESIAN_POINT ( 'NONE',  ( -10.46442989454075168, -10.46442989202483709, 13.65658308151907541 ) ) ;
#9318 = B_SPLINE_CURVE_WITH_KNOTS ( 'NONE', 3,
 ( #19515, #123, #5093, #8084, #16540, #6685, #14553, #14749, #8475, #16139, #438, #20, #11254, #229, #12860, #11559, #19303, #9672, #17936, #9865, #1824, #17733 ),
 .UNSPECIFIED., .F., .F.,
 ( 4, 2, 2, 2, 2, 2, 2, 2, 2, 2, 4 ),
 ( 0.008732568481177037031, 0.01468344170611684228, 0.02063431493105664927, 0.02658518815599645452, 0.03253606138093625977, 0.03551149799340617974, 0.03848693460587609277, 0.04443780783081591884, 0.05038868105575574491, 0.05336411766822565100, 0.05633955428069555710 ),
 .UNSPECIFIED. ) ;
#9319 = CIRCLE ( 'NONE', #178, 2.649999999999987477 ) ;
#9320 = VERTEX_POINT ( 'NONE', #17961 ) ;
#9321 = CARTESIAN_POINT ( 'NONE',  ( 16.55500000000001393, 0.000000000000000000, 2.500000000000000444 ) ) ;
#9322 = CARTESIAN_POINT ( 'NONE',  ( -16.62983158603122291, -6.888301780572501087, -19.69301249981969093 ) ) ;
#9323 = FACE_OUTER_BOUND ( 'NONE', #19401, .T. ) ;
#9324 = ORIENTED_EDGE ( 'NONE', *, *, #19442, .F. ) ;
#9325 = CARTESIAN_POINT ( 'NONE',  ( 19.99999999999999645, 62.46228066917787203, 18.86519267363478036 ) ) ;
#9326 = ORIENTED_EDGE ( 'NONE', *, *, #2056, .F. ) ;
#9327 = DIRECTION ( 'NONE',  ( 0.000000000000000000, 0.000000000000000000, -1.000000000000000000 ) ) ;
#9328 = CARTESIAN_POINT ( 'NONE',  ( -15.15000000000000036, 0.000000000000000000, 129.0000000000000000 ) ) ;
#9329 = ORIENTED_EDGE ( 'NONE', *, *, #18690, .T. ) ;
#9330 = ORIENTED_EDGE ( 'NONE', *, *, #16474, .F. ) ;
#9331 = CARTESIAN_POINT ( 'NONE',  ( 38.17990591115487575, -121.1390473681899351, -79.37944074850724974 ) ) ;
#9332 = VECTOR ( 'NONE', #1214, 1000.000000000000000 ) ;
#9333 = SURFACE_SIDE_STYLE ('',( #7844 ) ) ;
#9334 = DIRECTION ( 'NONE',  ( 1.000000000000000000, 0.000000000000000000, -0.000000000000000000 ) ) ;
#9335 = CIRCLE ( 'NONE', #8312, 65.24900000006525147 ) ;
#9336 = CARTESIAN_POINT ( 'NONE',  ( 19.99999999999999645, 59.31169354540775629, -27.19476070466793871 ) ) ;
#9337 = CARTESIAN_POINT ( 'NONE',  ( 9.474249097082498849, -6.330490858644140850, -1.473796499352572953 ) ) ;
#9338 = EDGE_CURVE ( 'NONE', #19615, #20567, #17032, .T. ) ;
#9339 = CARTESIAN_POINT ( 'NONE',  ( -6.358192987158591158, 4.248408730893245000, -22.30510624981969059 ) ) ;
#9340 = EDGE_CURVE ( 'NONE', #15390, #16808, #9916, .T. ) ;
#9341 = CARTESIAN_POINT ( 'NONE',  ( -6.165580000000000283, 0.000000000000000000, 0.000000000000000000 ) ) ;
#9342 = DIRECTION ( 'NONE',  ( 0.000000000000000000, 0.000000000000000000, 1.000000000000000000 ) ) ;
#9343 = DIRECTION ( 'NONE',  ( -0.000000000000000000, -0.000000000000000000, 1.000000000000000000 ) ) ;
#9344 = ORIENTED_EDGE ( 'NONE', *, *, #6504, .T. ) ;
#9345 = CARTESIAN_POINT ( 'NONE',  ( 24.99999999999999645, -85.00000000000000000, -1.040949779275250179E-14 ) ) ;
#9346 = AXIS2_PLACEMENT_3D ( 'NONE', #5504, #17075, #750 ) ;
#9347 = EDGE_LOOP ( 'NONE', ( #265, #19293, #11692, #8144 ) ) ;
#9348 = CARTESIAN_POINT ( 'NONE',  ( -6.888301784570738384, -16.62983158437509346, -13.35073749981969016 ) ) ;
#9349 = CARTESIAN_POINT ( 'NONE',  ( 14.87228507261736432, -15.53036221685708362, 73.48983352790762069 ) ) ;
#9350 = ADVANCED_FACE ( 'NONE', ( #7233 ), #10614, .T. ) ;
#9351 = VERTEX_POINT ( 'NONE', #7347 ) ;
#9352 = DIRECTION ( 'NONE',  ( 0.000000000000000000, 0.000000000000000000, 1.000000000000000000 ) ) ;
#9353 = AXIS2_PLACEMENT_3D ( 'NONE', #1970, #13204, #19653 ) ;
#9354 = ORIENTED_EDGE ( 'NONE', *, *, #8694, .T. ) ;
#9355 = AXIS2_PLACEMENT_3D ( 'NONE', #5391, #11859, #12258 ) ;
#9356 = CARTESIAN_POINT ( 'NONE',  ( 19.99999999999999645, 20.60847369613070512, -61.90898814327692889 ) ) ;
#9357 = FACE_OUTER_BOUND ( 'NONE', #19314, .T. ) ;
#9358 = DIRECTION ( 'NONE',  ( -1.000000000000000000, -0.000000000000000000, -0.000000000000000000 ) ) ;
#9359 = ORIENTED_EDGE ( 'NONE', *, *, #19111, .T. ) ;
#9360 = CARTESIAN_POINT ( 'NONE',  ( 6.359999999999997655, 7.000462221625649605E-15, 0.000000000000000000 ) ) ;
#9361 = AXIS2_PLACEMENT_3D ( 'NONE', #15165, #11982, #12187 ) ;
#9362 = DIRECTION ( 'NONE',  ( 0.000000000000000000, 0.000000000000000000, -1.000000000000000000 ) ) ;
#9363 = CARTESIAN_POINT ( 'NONE',  ( -15.25966316918061416, 10.19618095414378445, -20.12495624981969300 ) ) ;
#9364 = DIRECTION ( 'NONE',  ( -1.000000000000000000, 0.000000000000000000, 0.000000000000000000 ) ) ;
#9365 = EDGE_CURVE ( 'NONE', #14337, #14215, #1486, .T. ) ;
#9366 = AXIS2_PLACEMENT_3D ( 'NONE', #5233, #11700, #19948 ) ;
#9367 = AXIS2_PLACEMENT_3D ( 'NONE', #14730, #4874, #3474 ) ;
#9368 = CARTESIAN_POINT ( 'NONE',  ( -5.303300859536632217, -5.303300858261584594, 13.33317500018030977 ) ) ;
#9369 = EDGE_LOOP ( 'NONE', ( #5067, #2026, #14520, #12219 ) ) ;
#9370 = EDGE_CURVE ( 'NONE', #16482, #13364, #8566, .T. ) ;
#9371 = AXIS2_PLACEMENT_3D ( 'NONE', #9477, #19235, #14476 ) ;
#9372 = CARTESIAN_POINT ( 'NONE',  ( 1.084202172485504434E-14, 4.618802153517020059, -0.3572655899081733644 ) ) ;
#9373 = MECHANICAL_DESIGN_GEOMETRIC_PRESENTATION_REPRESENTATION (  '', ( #16807 ), #3289 ) ;
#9374 = EDGE_CURVE ( 'NONE', #5793, #11740, #6867, .T. ) ;
#9375 = CARTESIAN_POINT ( 'NONE',  ( 19.99999999999999645, 0.000000000000000000, 0.000000000000000000 ) ) ;
#9376 = VERTEX_POINT ( 'NONE', #15295 ) ;
#9377 = LINE ( 'NONE', #20697, #2022 ) ;
#9378 = DIRECTION ( 'NONE',  ( 0.000000000000000000, -0.2697967711570115057, -0.9629172873478029082 ) ) ;
#9379 = EDGE_CURVE ( 'NONE', #19446, #12867, #2143, .T. ) ;
#9380 = ORIENTED_EDGE ( 'NONE', *, *, #154, .F. ) ;
#9381 = CARTESIAN_POINT ( 'NONE',  ( 18.00000000043041126, 3.580422610670019434, -14.68598124981969022 ) ) ;
#9382 = AXIS2_PLACEMENT_3D ( 'NONE', #15577, #7741, #2864 ) ;
#9383 = LINE ( 'NONE', #3222, #17503 ) ;
#9384 = DIRECTION ( 'NONE',  ( 1.000000000000000000, 0.000000000000000000, 0.000000000000000000 ) ) ;
#9385 = VERTEX_POINT ( 'NONE', #784 ) ;
#9386 = CARTESIAN_POINT ( 'NONE',  ( 19.99999999999999645, 0.000000000000000000, 0.000000000000000000 ) ) ;
#9387 = ORIENTED_EDGE ( 'NONE', *, *, #20877, .F. ) ;
#9388 = CYLINDRICAL_SURFACE ( 'NONE', #3115, 27.60000000002759535 ) ;
#9389 = AXIS2_PLACEMENT_3D ( 'NONE', #8033, #3450, #16500 ) ;
#9390 = ORIENTED_EDGE ( 'NONE', *, *, #8017, .F. ) ;
#9391 = AXIS2_PLACEMENT_3D ( 'NONE', #16513, #8759, #5682 ) ;
#9392 = CIRCLE ( 'NONE', #8041, 10.00000000000000178 ) ;
#9393 = DIRECTION ( 'NONE',  ( -0.000000000000000000, -0.000000000000000000, 1.000000000000000000 ) ) ;
#9394 = EDGE_CURVE ( 'NONE', #13762, #16945, #14007, .T. ) ;
#9395 = CARTESIAN_POINT ( 'NONE',  ( 17.50000000000000355, 0.000000000000000000, 166.0000000000000000 ) ) ;
#9396 = AXIS2_PLACEMENT_3D ( 'NONE', #10360, #618, #1998 ) ;
#9397 = CARTESIAN_POINT ( 'NONE',  ( 5.663308646854342321, -13.67243654778935635, -1.342520581158454851 ) ) ;
#9398 = VERTEX_POINT ( 'NONE', #12224 ) ;
#9399 = LINE ( 'NONE', #2539, #20121 ) ;
#9400 = AXIS2_PLACEMENT_3D ( 'NONE', #20822, #17960, #11392 ) ;
#9401 = DIRECTION ( 'NONE',  ( 0.000000000000000000, -0.6310879443260433153, -0.7757112907044274586 ) ) ;
#9402 = VERTEX_POINT ( 'NONE', #674 ) ;
#9403 = CARTESIAN_POINT ( 'NONE',  ( 19.82535189207093040, -8.394204402731995529, 84.86463929178358967 ) ) ;
#9404 = AXIS2_PLACEMENT_3D ( 'NONE', #14304, #3264, #2960 ) ;
#9405 = DIRECTION ( 'NONE',  ( 0.000000000000000000, -0.8878852184023793281, 0.4600650377311439887 ) ) ;
#9406 = CARTESIAN_POINT ( 'NONE',  ( -31.74999999999995737, 0.000000000000000000, 0.000000000000000000 ) ) ;
#9407 = ORIENTED_EDGE ( 'NONE', *, *, #2649, .F. ) ;
#9408 = ADVANCED_FACE ( 'NONE', ( #13510 ), #12124, .F. ) ;
#9409 = DIRECTION ( 'NONE',  ( -0.000000000000000000, -0.000000000000000000, 1.000000000000000000 ) ) ;
#9410 = CARTESIAN_POINT ( 'NONE',  ( 50.00000000000000000, -159.9999999999999716, -53.99496054166690584 ) ) ;
#9411 = AXIS2_PLACEMENT_3D ( 'NONE', #774, #18365, #10525 ) ;
#9412 = EDGE_LOOP ( 'NONE', ( #11224, #2229 ) ) ;
#9413 = CARTESIAN_POINT ( 'NONE',  ( -22.55329027477439041, -4.616075264032610370, -88.80073566248103134 ) ) ;
#9414 = CARTESIAN_POINT ( 'NONE',  ( 56.98610214956094211, -164.9999999999999716, 84.54208835637712127 ) ) ;
#9415 = CARTESIAN_POINT ( 'NONE',  ( 17.99999999999999645, -2.163824016901520184E-09, -6.871049999819689447 ) ) ;
#9416 = SHAPE_REPRESENTATION ( 'worm', ( #12461 ), #7026 ) ;
#9417 = ORIENTED_EDGE ( 'NONE', *, *, #1722, .T. ) ;
#9418 = DIRECTION ( 'NONE',  ( -1.000000000000000000, 0.000000000000000000, 0.000000000000000000 ) ) ;
#9419 = CYLINDRICAL_SURFACE ( 'NONE', #7845, 27.60000000002760245 ) ;
#9420 = FACE_OUTER_BOUND ( 'NONE', #6030, .T. ) ;
#9421 = CARTESIAN_POINT ( 'NONE',  ( 6.250000000000054179, 10.82531754730546147, 43.00000000000000000 ) ) ;
#9422 = CARTESIAN_POINT ( 'NONE',  ( 40.00000000000036948, -100.0000000000005400, -51.99999999999864286 ) ) ;
#9423 = CARTESIAN_POINT ( 'NONE',  ( -12.72792205982780089, 12.72792206288791128, 0.9241750001803099579 ) ) ;
#9424 = CARTESIAN_POINT ( 'NONE',  ( 6.358192987158595599, -4.248408730893249441, -20.75270624981969192 ) ) ;
#9425 = ORIENTED_EDGE ( 'NONE', *, *, #2056, .T. ) ;
#9426 = DIRECTION ( 'NONE',  ( -1.000000000000000000, -0.000000000000000000, -0.000000000000000000 ) ) ;
#9427 = CARTESIAN_POINT ( 'NONE',  ( 11.17563879704981566, -2.222972771497744304, -28.03557850028681031 ) ) ;
#9428 = CARTESIAN_POINT ( 'NONE',  ( 50.00000000000000000, -164.9999999999999716, 90.00000000000001421 ) ) ;
#9429 = ORIENTED_EDGE ( 'NONE', *, *, #10672, .F. ) ;
#9430 = EDGE_CURVE ( 'NONE', #19301, #15433, #8941, .T. ) ;
#9431 = FACE_BOUND ( 'NONE', #7108, .T. ) ;
#9432 = DIRECTION ( 'NONE',  ( -1.000000000000000000, -0.000000000000000000, -0.000000000000000000 ) ) ;
#9433 = CARTESIAN_POINT ( 'NONE',  ( 8.899999999999900879, -10.82531754730554496, 40.00000000000000000 ) ) ;
#9434 = VERTEX_POINT ( 'NONE', #4168 ) ;
#9435 = LINE ( 'NONE', #6589, #10562 ) ;
#9436 = VERTEX_POINT ( 'NONE', #2271 ) ;
#9437 = CARTESIAN_POINT ( 'NONE',  ( 2.500000000000000000, 1.178949249685213863, -2.042000000000001148 ) ) ;
#9438 = CARTESIAN_POINT ( 'NONE',  ( 19.99999999999999645, 1.971042061629218356, -64.80882494896104618 ) ) ;
#9439 = VERTEX_POINT ( 'NONE', #15407 ) ;
#9440 = ORIENTED_EDGE ( 'NONE', *, *, #3165, .T. ) ;
#9441 = CARTESIAN_POINT ( 'NONE',  ( 0.000000000000000000, -65.23577793412346182, 1.313498510941474740 ) ) ;
#9442 = CARTESIAN_POINT ( 'NONE',  ( 19.99999999999999645, -5.762283366691622000, 64.99406197038668154 ) ) ;
#9443 = DIRECTION ( 'NONE',  ( -0.000000000000000000, -0.000000000000000000, -1.000000000000000000 ) ) ;
#9444 = CARTESIAN_POINT ( 'NONE',  ( 11.17563879731705789, -1.343450868547281933E-09, -11.78239024935257540 ) ) ;
#9445 = CARTESIAN_POINT ( 'NONE',  ( 2.870125743571137811, 6.929096493489625530, -20.24338749981969343 ) ) ;
#9446 = CARTESIAN_POINT ( 'NONE',  ( -12.50000000000000533, 0.000000000000000000, 169.0000000000000000 ) ) ;
#9447 = DIRECTION ( 'NONE',  ( 1.000000000000000000, -0.000000000000000000, -0.000000000000000000 ) ) ;
#9448 = LINE ( 'NONE', #1308, #11709 ) ;
#9449 = VERTEX_POINT ( 'NONE', #16677 ) ;
#9450 = LINE ( 'NONE', #7969, #9563 ) ;
#9451 = VERTEX_POINT ( 'NONE', #3734 ) ;
#9452 = CARTESIAN_POINT ( 'NONE',  ( -15.25966317163203279, -10.19618095047498052, -21.89214374981969158 ) ) ;
#9453 = CARTESIAN_POINT ( 'NONE',  ( 18.97564634267267181, -10.12806126886903613, 76.96678999104570096 ) ) ;
#9454 = ORIENTED_EDGE ( 'NONE', *, *, #13428, .T. ) ;
#9455 = CYLINDRICAL_SURFACE ( 'NONE', #14020, 72.00000000007199219 ) ;
#9456 = ORIENTED_EDGE ( 'NONE', *, *, #10669, .T. ) ;
#9457 = CARTESIAN_POINT ( 'NONE',  ( -4.248408730893246776, -6.358192987158592047, -5.811356249819692898 ) ) ;
#9458 = DIRECTION ( 'NONE',  ( 0.000000000000000000, 1.000000000000000000, 0.000000000000000000 ) ) ;
#9459 = DIRECTION ( 'NONE',  ( -1.000000000000000000, -0.000000000000000000, -0.000000000000000000 ) ) ;
#9460 = VERTEX_POINT ( 'NONE', #16783 ) ;
#9461 = CARTESIAN_POINT ( 'NONE',  ( 0.000000000000000000, 46.01927912072526539, 45.67597560296404424 ) ) ;
#9462 = ADVANCED_FACE ( 'NONE', ( #7125 ), #15512, .T. ) ;
#9463 = EDGE_CURVE ( 'NONE', #12885, #273, #11304, .T. ) ;
#9464 = CARTESIAN_POINT ( 'NONE',  ( -16.62983158437509701, 6.888301784570728614, -20.41948749981969158 ) ) ;
#9465 = CARTESIAN_POINT ( 'NONE',  ( 0.000000000000000000, 0.000000000000000000, -90.00000000000000000 ) ) ;
#9466 = CARTESIAN_POINT ( 'NONE',  ( -30.00000000000000000, 29.99999999999999289, -120.0000000000000142 ) ) ;
#9467 = EDGE_CURVE ( 'NONE', #9747, #20839, #17051, .T. ) ;
#9468 = ORIENTED_EDGE ( 'NONE', *, *, #3483, .F. ) ;
#9469 = AXIS2_PLACEMENT_3D ( 'NONE', #14997, #17878, #16271 ) ;
#9470 = CARTESIAN_POINT ( 'NONE',  ( 0.000000000000000000, 70.29359119158506530, -15.58239511117215415 ) ) ;
#9471 = DIRECTION ( 'NONE',  ( -1.000000000000000000, 0.000000000000000000, 0.000000000000000000 ) ) ;
#9472 = ORIENTED_EDGE ( 'NONE', *, *, #1702, .F. ) ;
#9473 = DIRECTION ( 'NONE',  ( 0.000000000000000000, 0.000000000000000000, -1.000000000000000000 ) ) ;
#9474 = CARTESIAN_POINT ( 'NONE',  ( -65.00002539999999840, 0.000000000000000000, 1.000000000000000000 ) ) ;
#9475 = ORIENTED_EDGE ( 'NONE', *, *, #11818, .F. ) ;
#9476 = CARTESIAN_POINT ( 'NONE',  ( -30.00000000000000000, 29.99999999999999289, -130.0000000000000000 ) ) ;
#9477 = CARTESIAN_POINT ( 'NONE',  ( 0.000000000000000000, 0.000000000000000000, 0.000000000000000000 ) ) ;
#9478 = CARTESIAN_POINT ( 'NONE',  ( 2.000000000000010658, -3.464101615137748169, -5.600000000000000533 ) ) ;
#9479 = VERTEX_POINT ( 'NONE', #18483 ) ;
#9480 = ADVANCED_FACE ( 'NONE', ( #3950 ), #8619, .T. ) ;
#9481 = CARTESIAN_POINT ( 'NONE',  ( 0.000000000000000000, -68.15657073222419626, -23.20952102120350347 ) ) ;
#9482 = ORIENTED_EDGE ( 'NONE', *, *, #8582, .F. ) ;
#9483 = CARTESIAN_POINT ( 'NONE',  ( 52.00000000000000000, -39.99999999999999289, 0.000000000000000000 ) ) ;
#9484 = EDGE_LOOP ( 'NONE', ( #5050, #11448, #12406, #18970 ) ) ;
#9485 = EDGE_CURVE ( 'NONE', #13866, #20036, #1563, .T. ) ;
#9486 = ADVANCED_FACE ( 'NONE', ( #4277 ), #9262, .F. ) ;
#9487 = CARTESIAN_POINT ( 'NONE',  ( 0.000000000000000000, 0.000000000000000000, 126.0000000000000000 ) ) ;
#9488 = ADVANCED_FACE ( 'NONE', ( #15725 ), #20595, .T. ) ;
#9489 = CARTESIAN_POINT ( 'NONE',  ( 0.000000000000000000, -53.26727847779503833, -48.44168704307686113 ) ) ;
#9490 = VECTOR ( 'NONE', #11218, 1000.000000000000000 ) ;
#9491 = CARTESIAN_POINT ( 'NONE',  ( -4.276731815070949239, -10.32494394706616347, 19.43792225064743562 ) ) ;
#9492 = EDGE_LOOP ( 'NONE', ( #8315, #18711, #12702, #19518 ) ) ;
#9493 = CARTESIAN_POINT ( 'NONE',  ( -39.99999999999999289, -40.00000000000000000, -120.0000000000000142 ) ) ;
#9494 = DIRECTION ( 'NONE',  ( 0.000000000000000000, 0.7308359642781252496, -0.6825531432186529024 ) ) ;
#9495 = ORIENTED_EDGE ( 'NONE', *, *, #5070, .F. ) ;
#9496 = CARTESIAN_POINT ( 'NONE',  ( 16.80839512764391586, -13.42119425201006422, 80.75675983441298911 ) ) ;
#9497 = CARTESIAN_POINT ( 'NONE',  ( 19.99999999999999645, -64.44931368725514176, -10.18420179740675380 ) ) ;
#9498 = AXIS2_PLACEMENT_3D ( 'NONE', #5215, #11784, #18046 ) ;
#9499 = CARTESIAN_POINT ( 'NONE',  ( -7.459310946700270506E-14, -4.618802153517020948, -5.242734410091827613 ) ) ;
#9500 = EDGE_CURVE ( 'NONE', #1825, #100, #4875, .T. ) ;
#9501 = EDGE_CURVE ( 'NONE', #1075, #8470, #19421, .T. ) ;
#9502 = ORIENTED_EDGE ( 'NONE', *, *, #19562, .T. ) ;
#9503 = CARTESIAN_POINT ( 'NONE',  ( -3.344563996438217224, -2.687817229851499068, -0.1586754815285013609 ) ) ;
#9504 = CARTESIAN_POINT ( 'NONE',  ( -2.060000000000000941, 2.522772406243548923E-16, -0.3080913168122707546 ) ) ;
#9505 = VECTOR ( 'NONE', #18683, 1000.000000000000000 ) ;
#9506 = ORIENTED_EDGE ( 'NONE', *, *, #16207, .F. ) ;
#9507 = CARTESIAN_POINT ( 'NONE',  ( -30.00000000000000000, -85.00000000000000000, -1.040949779275250179E-14 ) ) ;
#9508 = CARTESIAN_POINT ( 'NONE',  ( 2.500000000000000000, 0.000000000000000000, 0.000000000000000000 ) ) ;
#9509 = FACE_OUTER_BOUND ( 'NONE', #8221, .T. ) ;
#9510 = EDGE_CURVE ( 'NONE', #20241, #7282, #7985, .T. ) ;
#9511 = ORIENTED_EDGE ( 'NONE', *, *, #16233, .F. ) ;
#9512 = LINE ( 'NONE', #1477, #10056 ) ;
#9513 = LINE ( 'NONE', #17684, #16644 ) ;
#9514 = CARTESIAN_POINT ( 'NONE',  ( -6.359999999999999432, 10.52400000000000091, 0.000000000000000000 ) ) ;
#9515 = CARTESIAN_POINT ( 'NONE',  ( 1.071320128151698542E-30, -5.832187760079096936E-15, 74.99999999999998579 ) ) ;
#9516 = CARTESIAN_POINT ( 'NONE',  ( -15.25966317163203456, -10.19618095047498230, -10.56254374981969413 ) ) ;
#9517 = DIRECTION ( 'NONE',  ( -1.836909530733573776E-16, 1.000000000000000000, 0.000000000000000000 ) ) ;
#9518 = AXIS2_PLACEMENT_3D ( 'NONE', #6248, #14002, #3067 ) ;
#9519 = CARTESIAN_POINT ( 'NONE',  ( 19.99999999999999645, 28.84646472442533494, -58.52617768068405013 ) ) ;
#9520 = CARTESIAN_POINT ( 'NONE',  ( -4.276731815070945686, -10.32494394706615637, -25.38479725028680889 ) ) ;
#9521 = FACE_OUTER_BOUND ( 'NONE', #6632, .T. ) ;
#9522 = ORIENTED_EDGE ( 'NONE', *, *, #7364, .F. ) ;
#9523 = CARTESIAN_POINT ( 'NONE',  ( 4.999999999999997335, 0.000000000000000000, 0.000000000000000000 ) ) ;
#9524 = FACE_BOUND ( 'NONE', #7999, .T. ) ;
#9525 = PLANE ( 'NONE',  #18181 ) ;
#9526 = EDGE_LOOP ( 'NONE', ( #5422, #6193, #17558, #19256 ) ) ;
#9527 = CARTESIAN_POINT ( 'NONE',  ( 10.00000000000000178, -160.0000000000000000, 70.00000000000000000 ) ) ;
#9528 = AXIS2_PLACEMENT_3D ( 'NONE', #4411, #10681, #2628 ) ;
#9529 = ORIENTED_EDGE ( 'NONE', *, *, #20237, .F. ) ;
#9530 = CARTESIAN_POINT ( 'NONE',  ( 31.95495987947095173, -34.31614948441001900, -72.06256082998474710 ) ) ;
#9531 = DIRECTION ( 'NONE',  ( 0.000000000000000000, 0.000000000000000000, 1.000000000000000000 ) ) ;
#9532 = ORIENTED_EDGE ( 'NONE', *, *, #18377, .F. ) ;
#9533 = CIRCLE ( 'NONE', #19030, 3.199999999999994404 ) ;
#9534 = ORIENTED_EDGE ( 'NONE', *, *, #5097, .F. ) ;
#9535 = CARTESIAN_POINT ( 'NONE',  ( -6.359999999999995879, -10.85999999999998877, 1.329966423874024955E-15 ) ) ;
#9536 =( REPRESENTATION_RELATIONSHIP ('NONE','NONE', #13739, #12383 ) REPRESENTATION_RELATIONSHIP_WITH_TRANSFORMATION ( #7586 )SHAPE_REPRESENTATION_RELATIONSHIP( ) );
#9537 = CARTESIAN_POINT ( 'NONE',  ( -30.00000000000000000, -42.57363661491096707, -121.3828884801879155 ) ) ;
#9538 = EDGE_CURVE ( 'NONE', #6065, #3008, #3007, .T. ) ;
#9539 = EDGE_CURVE ( 'NONE', #17751, #3623, #5889, .T. ) ;
#9540 = FACE_OUTER_BOUND ( 'NONE', #6738, .T. ) ;
#9541 = CARTESIAN_POINT ( 'NONE',  ( 9.474249098604511587, 6.330490856366296271, -12.66598399935257468 ) ) ;
#9542 = AXIS2_PLACEMENT_3D ( 'NONE', #12464, #2108, #2008 ) ;
#9543 = AXIS2_PLACEMENT_3D ( 'NONE', #15593, #7430, #6055 ) ;
#9544 = CARTESIAN_POINT ( 'NONE',  ( 7.499999999820660790, -1.491842756249031954, -18.18166874981969272 ) ) ;
#9545 = DIRECTION ( 'NONE',  ( 0.000000000000000000, 0.000000000000000000, -1.000000000000000000 ) ) ;
#9546 = CIRCLE ( 'NONE', #15308, 65.24900000006525147 ) ;
#9547 = CARTESIAN_POINT ( 'NONE',  ( 48.35276434571220250, -3.649167310370820871, 90.00000000000000000 ) ) ;
#9548 = DIRECTION ( 'NONE',  ( 1.000000000000000000, 0.000000000000000000, 0.000000000000000000 ) ) ;
#9549 = ORIENTED_EDGE ( 'NONE', *, *, #11938, .T. ) ;
#9550 = CYLINDRICAL_SURFACE ( 'NONE', #13287, 27.60000000002760245 ) ;
#9551 = VERTEX_POINT ( 'NONE', #2691 ) ;
#9552 = CARTESIAN_POINT ( 'NONE',  ( 15.25966317163202746, 10.19618095047498407, -17.17964374981969300 ) ) ;
#9553 = FACE_OUTER_BOUND ( 'NONE', #20631, .T. ) ;
#9554 = ORIENTED_EDGE ( 'NONE', *, *, #12244, .F. ) ;
#9555 = DIRECTION ( 'NONE',  ( 0.000000000000000000, 0.000000000000000000, -1.000000000000000000 ) ) ;
#9556 = ORIENTED_EDGE ( 'NONE', *, *, #14171, .T. ) ;
#9557 = CARTESIAN_POINT ( 'NONE',  ( 0.000000000000000000, 59.36728637278075382, -40.73727173906726762 ) ) ;
#9558 = PLANE ( 'NONE',  #17869 ) ;
#9559 = CARTESIAN_POINT ( 'NONE',  ( -4.248408729364577141, 6.358192988180014993, -2.866043749819691122 ) ) ;
#9560 = ORIENTED_EDGE ( 'NONE', *, *, #9106, .T. ) ;
#9561 = CARTESIAN_POINT ( 'NONE',  ( 19.99999999999999645, -28.84646472442495480, 58.52617768068423487 ) ) ;
#9562 = CIRCLE ( 'NONE', #10235, 18.00000000000000000 ) ;
#9563 = VECTOR ( 'NONE', #12851, 1000.000000000000000 ) ;
#9564 = AXIS2_PLACEMENT_3D ( 'NONE', #15333, #5680, #16600 ) ;
#9565 = FACE_OUTER_BOUND ( 'NONE', #7405, .T. ) ;
#9566 = DIRECTION ( 'NONE',  ( 0.000000000000000000, 0.000000000000000000, -1.000000000000000000 ) ) ;
#9567 = EDGE_CURVE ( 'NONE', #18058, #19863, #20076, .T. ) ;
#9568 = CARTESIAN_POINT ( 'NONE',  ( 5.303300858261583706, -5.303300859536632217, 10.97692500018030870 ) ) ;
#9569 = AXIS2_PLACEMENT_3D ( 'NONE', #15329, #611, #13637 ) ;
#9570 = ORIENTED_EDGE ( 'NONE', *, *, #4167, .T. ) ;
#9571 = CARTESIAN_POINT ( 'NONE',  ( 19.99999999999999645, 49.77519642624007901, 42.18840861821802690 ) ) ;
#9572 = CARTESIAN_POINT ( 'NONE',  ( 7.500000000000005329, -1.491842755816077393, -2.491768749912207870 ) ) ;
#9573 = ORIENTED_EDGE ( 'NONE', *, *, #19434, .F. ) ;
#9574 = AXIS2_PLACEMENT_3D ( 'NONE', #1876, #8642, #5047 ) ;
#9575 = DIRECTION ( 'NONE',  ( 0.000000000000000000, -0.3984010898462297390, -0.9172113015054581542 ) ) ;
#9576 = DIRECTION ( 'NONE',  ( 0.000000000000000000, -7.039457583666959814E-15, 1.000000000000000000 ) ) ;
#9577 = ADVANCED_FACE ( 'NONE', ( #4381 ), #14358, .T. ) ;
#9578 = AXIS2_PLACEMENT_3D ( 'NONE', #3061, #4552, #20753 ) ;
#9579 = PRESENTATION_LAYER_ASSIGNMENT (  '', '', ( #18720 ) ) ;
#9580 = ORIENTED_EDGE ( 'NONE', *, *, #12903, .T. ) ;
#9581 = DIRECTION ( 'NONE',  ( -1.000000000000000000, 0.000000000000000000, 0.000000000000000000 ) ) ;
#9582 = CIRCLE ( 'NONE', #14237, 27.60000000002759535 ) ;
#9583 = DIRECTION ( 'NONE',  ( 8.673617379884035472E-17, -1.000000000000000000, 0.000000000000000000 ) ) ;
#9584 = CARTESIAN_POINT ( 'NONE',  ( -6.165580000000000283, 9.226011372524489750E-16, -7.500000000000000000 ) ) ;
#9585 = ORIENTED_EDGE ( 'NONE', *, *, #13628, .T. ) ;
#9586 = CARTESIAN_POINT ( 'NONE',  ( 50.00000000000000000, -1.326995226329880762, -84.99999999999998579 ) ) ;
#9587 = VERTEX_POINT ( 'NONE', #9153 ) ;
#9588 = CARTESIAN_POINT ( 'NONE',  ( -10.00000000000000000, 0.000000000000000000, 0.000000000000000000 ) ) ;
#9589 = ORIENTED_EDGE ( 'NONE', *, *, #4292, .F. ) ;
#9590 = EDGE_CURVE ( 'NONE', #6246, #19691, #3183, .T. ) ;
#9591 = AXIS2_PLACEMENT_3D ( 'NONE', #7203, #552, #13690 ) ;
#9592 = DIRECTION ( 'NONE',  ( 0.000000000000000000, 0.5195839500354344498, -0.8544194045464880150 ) ) ;
#9593 = AXIS2_PLACEMENT_3D ( 'NONE', #8008, #20928, #15746 ) ;
#9594 = AXIS2_PLACEMENT_3D ( 'NONE', #464, #771, #15083 ) ;
#9595 = DIRECTION ( 'NONE',  ( -0.000000000000000000, -0.000000000000000000, 1.000000000000000000 ) ) ;
#9596 = CARTESIAN_POINT ( 'NONE',  ( 8.382925371439633011, 12.54593441562640876, -14.00736433115846324 ) ) ;
#9597 = ORIENTED_EDGE ( 'NONE', *, *, #4940, .F. ) ;
#9598 = DIRECTION ( 'NONE',  ( 1.000000000000000000, 1.836909530733573776E-16, 0.000000000000000000 ) ) ;
#9599 = LINE ( 'NONE', #1756, #13638 ) ;
#9600 = ORIENTED_EDGE ( 'NONE', *, *, #16346, .T. ) ;
#9601 = CIRCLE ( 'NONE', #10276, 72.00000000007199219 ) ;
#9602 = CARTESIAN_POINT ( 'NONE',  ( -2.904526653654485813, -21.31518795036016201, 76.12711593406372401 ) ) ;
#9603 = CIRCLE ( 'NONE', #470, 27.60000000002760245 ) ;
#9604 = EDGE_CURVE ( 'NONE', #1518, #15789, #7211, .T. ) ;
#9605 = CIRCLE ( 'NONE', #16040, 5.000000000000000888 ) ;
#9606 = EDGE_CURVE ( 'NONE', #10438, #17156, #1424, .T. ) ;
#9607 = CARTESIAN_POINT ( 'NONE',  ( -10.00000000000000000, 0.000000000000000000, 0.000000000000000000 ) ) ;
#9608 = CARTESIAN_POINT ( 'NONE',  ( 19.99999999999999645, -68.15657073222450890, 23.20952102120258331 ) ) ;
#9609 = LINE ( 'NONE', #12900, #11724 ) ;
#9610 = AXIS2_PLACEMENT_3D ( 'NONE', #28, #11373, #130 ) ;
#9611 = CIRCLE ( 'NONE', #11961, 2.649999999999999467 ) ;
#9612 = ORIENTED_EDGE ( 'NONE', *, *, #8721, .T. ) ;
#9613 = EDGE_CURVE ( 'NONE', #18213, #349, #7914, .T. ) ;
#9614 = FACE_OUTER_BOUND ( 'NONE', #19299, .T. ) ;
#9615 = PLANE ( 'NONE',  #2240 ) ;
#9616 = EDGE_CURVE ( 'NONE', #16343, #13609, #16042, .T. ) ;
#9617 = EDGE_LOOP ( 'NONE', ( #5882, #9187, #12332, #17418 ) ) ;
#9618 = CARTESIAN_POINT ( 'NONE',  ( -11.59853973546238315, -19.87550760251307835, -76.83006856037964383 ) ) ;
#9619 = CARTESIAN_POINT ( 'NONE',  ( 19.99999999999999645, -20.34307325858738835, -69.06634035770328239 ) ) ;
#9620 = DIRECTION ( 'NONE',  ( -1.648349939164583989E-16, 1.000000000000000000, 0.000000000000000000 ) ) ;
#9621 = CIRCLE ( 'NONE', #11316, 2.099999999999990763 ) ;
#9622 = ORIENTED_EDGE ( 'NONE', *, *, #9100, .T. ) ;
#9623 = DIRECTION ( 'NONE',  ( -1.000000000000000000, 0.000000000000000000, 0.000000000000000000 ) ) ;
#9624 = VECTOR ( 'NONE', #18937, 1000.000000000000000 ) ;
#9625 = LINE ( 'NONE', #10112, #8509 ) ;
#9626 = FACE_OUTER_BOUND ( 'NONE', #5523, .T. ) ;
#9627 = DIRECTION ( 'NONE',  ( 6.982962677686266711E-15, 0.000000000000000000, -1.000000000000000000 ) ) ;
#9628 = ADVANCED_FACE ( 'NONE', ( #1112, #12866 ), #14862, .T. ) ;
#9629 = CARTESIAN_POINT ( 'NONE',  ( -12.72792206288791483, -12.72792205982780089, -20.28207499981969519 ) ) ;
#9630 = B_SPLINE_CURVE_WITH_KNOTS ( 'NONE', 3,
 ( #10303, #13387, #11679, #18247, #3513, #18147, #5512, #6790, #16549, #10092, #8392, #5409, #7102, #243, #3714, #11573, #10410, #2033, #18458, #2244, #8484, #13175 ),
 .UNSPECIFIED., .F., .F.,
 ( 4, 2, 2, 2, 2, 2, 2, 2, 2, 2, 4 ),
 ( 0.01090777686127726055, 0.01377645490973365520, 0.01664513295819005159, 0.01807947198241826800, 0.01951381100664648441, 0.02238248905510294498, 0.02525116710355940555, 0.02668550612778763237, 0.02811984515201586265, 0.03098852320047232323, 0.03385720124892877686 ),
 .UNSPECIFIED. ) ;
#9631 = EDGE_CURVE ( 'NONE', #3467, #2027, #12314, .T. ) ;
#9632 = ORIENTED_EDGE ( 'NONE', *, *, #13950, .T. ) ;
#9633 = AXIS2_PLACEMENT_3D ( 'NONE', #11080, #5984, #14056 ) ;
#9634 = DIRECTION ( 'NONE',  ( -0.000000000000000000, -0.000000000000000000, 1.000000000000000000 ) ) ;
#9635 = CARTESIAN_POINT ( 'NONE',  ( 0.000000000000000000, -27.62776854598897813, 58.65812137498992485 ) ) ;
#9636 = CARTESIAN_POINT ( 'NONE',  ( 12.54593441562639988, -8.382925371439625906, -7.844198168480929212 ) ) ;
#9637 = EDGE_CURVE ( 'NONE', #20917, #15524, #6883, .T. ) ;
#9638 = CARTESIAN_POINT ( 'NONE',  ( 10.00000000000000178, -164.9999999999999716, 70.00000000000000000 ) ) ;
#9639 = AXIS2_PLACEMENT_3D ( 'NONE', #8481, #3504, #14558 ) ;
#9640 = ADVANCED_FACE ( 'NONE', ( #5011 ), #8389, .T. ) ;
#9641 = ORIENTED_EDGE ( 'NONE', *, *, #14974, .F. ) ;
#9642 = DIRECTION ( 'NONE',  ( -1.000000000000000000, -0.000000000000000000, 0.000000000000000000 ) ) ;
#9643 = DIRECTION ( 'NONE',  ( 0.000000000000000000, 0.000000000000000000, -1.000000000000000000 ) ) ;
#9644 = DIRECTION ( 'NONE',  ( -0.000000000000000000, -0.000000000000000000, 1.000000000000000000 ) ) ;
#9645 = VERTEX_POINT ( 'NONE', #3507 ) ;
#9646 = CARTESIAN_POINT ( 'NONE',  ( 19.99999999999999645, -61.72688495901628869, 19.84591825363989415 ) ) ;
#9647 = EDGE_LOOP ( 'NONE', ( #6085, #16166 ) ) ;
#9648 = AXIS2_PLACEMENT_3D ( 'NONE', #18995, #4582, #19210 ) ;
#9649 = FACE_BOUND ( 'NONE', #14420, .T. ) ;
#9650 = CARTESIAN_POINT ( 'NONE',  ( 30.00000000000000000, -30.00000000000000711, -58.09475019311124555 ) ) ;
#9651 = ORIENTED_EDGE ( 'NONE', *, *, #12128, .F. ) ;
#9652 = ORIENTED_EDGE ( 'NONE', *, *, #2948, .F. ) ;
#9653 = CARTESIAN_POINT ( 'NONE',  ( 45.22159793441012710, -8.673994507468377080, 78.07221698934969822 ) ) ;
#9654 = FILL_AREA_STYLE_COLOUR ( '', #18864 ) ;
#9655 = DIRECTION ( 'NONE',  ( 0.000000000000000000, -0.5000000000000013323, -0.8660254037844380415 ) ) ;
#9656 = EDGE_CURVE ( 'NONE', #16131, #3271, #17942, .T. ) ;
#9657 = CARTESIAN_POINT ( 'NONE',  ( -4.248408729364580694, 6.358192988180020322, 12.82385625018031483 ) ) ;
#9658 = CIRCLE ( 'NONE', #15741, 2.099999999999997868 ) ;
#9659 = CARTESIAN_POINT ( 'NONE',  ( 9.474249097082495297, -6.330490858644137298, 0.8284839997131990819 ) ) ;
#9660 = DIRECTION ( 'NONE',  ( 0.000000000000000000, 0.000000000000000000, -1.000000000000000000 ) ) ;
#9661 =( BOUNDED_CURVE ( )  B_SPLINE_CURVE ( 2, ( #12394, #9210, #2542, #5595, #7402, #10807, #18436, #20445, #10593, #15564, #13879, #2423, #8884, #3899, #7185, #12077, #13778 ),
 .UNSPECIFIED., .F., .F. ) 
 B_SPLINE_CURVE_WITH_KNOTS ( ( 3, 2, 2, 2, 2, 2, 2, 2, 3 ),
 ( 0.1000000000038511888, 0.1125000000038511860, 0.1250000000038511694, 0.1375000000038511805, 0.1500000000038511638, 0.1625000000038511749, 0.1750000000038511583, 0.1875000000038511694, 0.2000000000038511805 ),
 .UNSPECIFIED. ) 
 CURVE ( )  GEOMETRIC_REPRESENTATION_ITEM ( )  RATIONAL_B_SPLINE_CURVE ( ( 0.9999999999940800688, 0.9807852804091503618, 1.000000000000000000, 0.9807852804032304306, 1.000000000000000000, 0.9807852804032304306, 1.000000000000000000, 0.9807852804032304306, 1.000000000000000000, 0.9807852804032304306, 1.000000000000000000, 0.9807852804032304306, 1.000000000000000000, 0.9807852804032304306, 1.000000000000000000, 0.9807852803973104994, 1.000000000005919931 ) ) 
 REPRESENTATION_ITEM ( '' )  );
#9662 = DIRECTION ( 'NONE',  ( -0.000000000000000000, 0.000000000000000000, -1.000000000000000000 ) ) ;
#9663 = DIRECTION ( 'NONE',  ( 0.000000000000000000, 0.000000000000000000, 1.000000000000000000 ) ) ;
#9664 = EDGE_LOOP ( 'NONE', ( #18747, #6141, #7215, #8919 ) ) ;
#9665 = DIRECTION ( 'NONE',  ( -1.000000000000000000, 0.000000000000000000, -0.000000000000000000 ) ) ;
#9666 = ORIENTED_EDGE ( 'NONE', *, *, #11190, .T. ) ;
#9667 = CARTESIAN_POINT ( 'NONE',  ( -12.72792206288791128, -12.72792205982779912, 7.992925000180314044 ) ) ;
#9668 = CYLINDRICAL_SURFACE ( 'NONE', #15052, 80.00000000000000000 ) ;
#9669 = VERTEX_POINT ( 'NONE', #8182 ) ;
#9670 = CARTESIAN_POINT ( 'NONE',  ( 19.99999999999999645, -64.44931368725528387, 10.18420179740584608 ) ) ;
#9671 = ORIENTED_EDGE ( 'NONE', *, *, #3184, .F. ) ;
#9672 = CARTESIAN_POINT ( 'NONE',  ( 30.18965574827983289, -44.98719419906327488, 71.43126268043587856 ) ) ;
#9673 = ADVANCED_FACE ( 'NONE', ( #16244 ), #2031, .T. ) ;
#9674 = EDGE_LOOP ( 'NONE', ( #18128, #18626, #8611, #2879 ) ) ;
#9675 = ORIENTED_EDGE ( 'NONE', *, *, #2765, .F. ) ;
#9676 = CARTESIAN_POINT ( 'NONE',  ( 10.00000000000000178, -164.9999999999999716, -73.20000000000000284 ) ) ;
#9677 = AXIS2_PLACEMENT_3D ( 'NONE', #9266, #15929, #1223 ) ;
#9678 = DIRECTION ( 'NONE',  ( 0.000000000000000000, 0.000000000000000000, -1.000000000000000000 ) ) ;
#9679 = CARTESIAN_POINT ( 'NONE',  ( -21.50000000000000000, 2.632990618166809235E-15, 84.99999999999998579 ) ) ;
#9680 = CARTESIAN_POINT ( 'NONE',  ( 0.000000000000000000, -1.178949249685214307, 2.042000000000001592 ) ) ;
#9681 = VERTEX_POINT ( 'NONE', #5099 ) ;
#9682 = DIRECTION ( 'NONE',  ( 0.000000000000000000, -0.8169698930104469792, 0.5766803221148600889 ) ) ;
#9683 = VECTOR ( 'NONE', #12814, 1000.000000000000000 ) ;
#9684 = CARTESIAN_POINT ( 'NONE',  ( 6.929096493489630859, -2.870125743571144472, -2.197237499819686857 ) ) ;
#9685 = DIRECTION ( 'NONE',  ( -1.000000000000000000, 0.000000000000000000, 0.000000000000000000 ) ) ;
#9686 = DIRECTION ( 'NONE',  ( 0.000000000000000000, 0.000000000000000000, 1.000000000000000000 ) ) ;
#9687 = CIRCLE ( 'NONE', #1573, 2.099999999999990763 ) ;
#9688 = EDGE_LOOP ( 'NONE', ( #2390, #6044, #11278, #15110 ) ) ;
#9689 = DIRECTION ( 'NONE',  ( 0.000000000000000000, 0.000000000000000000, 1.000000000000000000 ) ) ;
#9690 = CARTESIAN_POINT ( 'NONE',  ( 0.000000000000000000, 0.000000000000000000, -5.600000000000000533 ) ) ;
#9691 = DIRECTION ( 'NONE',  ( 0.000000000000000000, 0.000000000000000000, 1.000000000000000000 ) ) ;
#9692 = ORIENTED_EDGE ( 'NONE', *, *, #4006, .F. ) ;
#9693 = CYLINDRICAL_SURFACE ( 'NONE', #12975, 27.60000000002759890 ) ;
#9694 = VERTEX_POINT ( 'NONE', #238 ) ;
#9695 = CARTESIAN_POINT ( 'NONE',  ( -62.49999999999999289, -120.0000000000000142, 5.000000000000000000 ) ) ;
#9696 = EDGE_CURVE ( 'NONE', #4938, #12626, #12967, .T. ) ;
#9697 = VERTEX_POINT ( 'NONE', #14966 ) ;
#9698 = AXIS2_PLACEMENT_3D ( 'NONE', #9776, #13379, #1726 ) ;
#9699 = DIRECTION ( 'NONE',  ( 0.000000000000000000, 0.000000000000000000, 1.000000000000000000 ) ) ;
#9700 = VECTOR ( 'NONE', #6910, 1000.000000000000000 ) ;
#9701 = CIRCLE ( 'NONE', #20528, 65.24900000006525147 ) ;
#9702 = LINE ( 'NONE', #14683, #5514 ) ;
#9703 = CARTESIAN_POINT ( 'NONE',  ( -11.17563879731705789, 1.343452237168309506E-09, 21.20510975064742709 ) ) ;
#9704 = ORIENTED_EDGE ( 'NONE', *, *, #7120, .T. ) ;
#9705 = DIRECTION ( 'NONE',  ( 0.000000000000000000, 0.000000000000000000, 1.000000000000000000 ) ) ;
#9706 = VECTOR ( 'NONE', #16031, 1000.000000000000000 ) ;
#9707 = FACE_OUTER_BOUND ( 'NONE', #10310, .T. ) ;
#9708 = EDGE_LOOP ( 'NONE', ( #4038, #18450, #7242, #11561 ) ) ;
#9709 = CARTESIAN_POINT ( 'NONE',  ( -0.6543461111163950683, -4.241015250120822699, -0.1391502195351546900 ) ) ;
#9710 = VECTOR ( 'NONE', #16839, 1000.000000000000000 ) ;
#9711 = DIRECTION ( 'NONE',  ( 0.000000000000000000, -1.000000000000000000, 0.000000000000000000 ) ) ;
#9712 = DIRECTION ( 'NONE',  ( -8.673617379884035472E-17, 1.000000000000000000, 0.000000000000000000 ) ) ;
#9713 = DIRECTION ( 'NONE',  ( 1.202124453834178339E-10, 1.000000000000000000, 8.650973189387494397E-26 ) ) ;
#9714 = CIRCLE ( 'NONE', #9391, 65.24900000006525147 ) ;
#9715 = ORIENTED_EDGE ( 'NONE', *, *, #13859, .T. ) ;
#9716 = DIRECTION ( 'NONE',  ( -1.000000000000000000, 0.000000000000000000, 0.000000000000000000 ) ) ;
#9717 = VERTEX_POINT ( 'NONE', #11675 ) ;
#9718 = CARTESIAN_POINT ( 'NONE',  ( -14.03392052762769993, -18.23657722200194087, -77.70237658995378638 ) ) ;
#9719 = DIRECTION ( 'NONE',  ( 1.000000000000000000, 0.000000000000000000, 0.000000000000000000 ) ) ;
#9720 = CARTESIAN_POINT ( 'NONE',  ( -2.163827323447877821E-09, -17.99999999999999645, -23.36479999981969158 ) ) ;
#9721 = AXIS2_PLACEMENT_3D ( 'NONE', #15994, #16299, #194 ) ;
#9722 = VERTEX_POINT ( 'NONE', #19729 ) ;
#9723 = FACE_OUTER_BOUND ( 'NONE', #8477, .T. ) ;
#9724 = EDGE_CURVE ( 'NONE', #13652, #9255, #17849, .T. ) ;
#9725 = CIRCLE ( 'NONE', #4990, 40.00000000000000000 ) ;
#9726 = EDGE_CURVE ( 'NONE', #10201, #15185, #8283, .T. ) ;
#9727 = DIRECTION ( 'NONE',  ( 0.000000000000000000, 0.000000000000000000, -1.000000000000000000 ) ) ;
#9728 = CARTESIAN_POINT ( 'NONE',  ( 15.25966316918061771, -10.19618095414378800, -13.50785624981969235 ) ) ;
#9730 = ORIENTED_EDGE ( 'NONE', *, *, #14560, .T. ) ;
#9729 = AXIS2_PLACEMENT_3D ( 'NONE', #6164, #18907, #1527 ) ;
#9731 = AXIS2_PLACEMENT_3D ( 'NONE', #11716, #19454, #276 ) ;
#9732 = DIRECTION ( 'NONE',  ( -1.000000000000000000, -0.000000000000000000, -0.000000000000000000 ) ) ;
#9733 = ADVANCED_FACE ( 'NONE', ( #13172 ), #16148, .F. ) ;
#9734 = CARTESIAN_POINT ( 'NONE',  ( 19.99999999999999645, -63.48283426024828202, -33.96954156735433372 ) ) ;
#9735 = CARTESIAN_POINT ( 'NONE',  ( -5.663308646854335215, 13.67243654778934925, -2.248104418480928235 ) ) ;
#9736 = ORIENTED_EDGE ( 'NONE', *, *, #17964, .F. ) ;
#9737 = CIRCLE ( 'NONE', #15148, 65.24900000006525147 ) ;
#9738 = ORIENTED_EDGE ( 'NONE', *, *, #154, .T. ) ;
#9739 = CARTESIAN_POINT ( 'NONE',  ( -17.50000000000000355, 2.143131898507868643E-15, 126.0000000000000000 ) ) ;
#9740 = VECTOR ( 'NONE', #16890, 1000.000000000000000 ) ;
#9741 = CARTESIAN_POINT ( 'NONE',  ( 0.000000000000000000, 0.000000000000000000, -90.00000000000000000 ) ) ;
#9742 = CARTESIAN_POINT ( 'NONE',  ( 35.69831387705275461, -23.59893667096173431, 69.72867780164767737 ) ) ;
#9743 = VERTEX_POINT ( 'NONE', #19420 ) ;
#9744 = EDGE_CURVE ( 'NONE', #13498, #13788, #5209, .T. ) ;
#9745 = CARTESIAN_POINT ( 'NONE',  ( -10.00000000000000000, 0.000000000000000000, 0.000000000000000000 ) ) ;
#9746 = AXIS2_PLACEMENT_3D ( 'NONE', #13128, #14607, #3563 ) ;
#9747 = VERTEX_POINT ( 'NONE', #18144 ) ;
#9748 = CARTESIAN_POINT ( 'NONE',  ( 50.00000000000000000, -139.6410161513775563, 89.99999999999998579 ) ) ;
#9749 = CARTESIAN_POINT ( 'NONE',  ( -15.25966317163202923, -10.19618095047497874, 15.80785625018031304 ) ) ;
#9750 = ORIENTED_EDGE ( 'NONE', *, *, #16747, .F. ) ;
#9751 = VERTEX_POINT ( 'NONE', #6480 ) ;
#9752 = CARTESIAN_POINT ( 'NONE',  ( 48.84346035822958498, -2.517149734616030088, 83.65074274608480209 ) ) ;
#9753 = ADVANCED_FACE ( 'NONE', ( #9779, #8091 ), #3213, .F. ) ;
#9754 = EDGE_CURVE ( 'NONE', #13162, #8404, #20439, .T. ) ;
#9755 = DIRECTION ( 'NONE',  ( -1.000000000000000000, 0.000000000000000000, 0.000000000000000000 ) ) ;
#9756 = FACE_OUTER_BOUND ( 'NONE', #3580, .T. ) ;
#9757 = DIRECTION ( 'NONE',  ( 0.000000000000000000, 0.000000000000000000, 1.000000000000000000 ) ) ;
#9758 = CARTESIAN_POINT ( 'NONE',  ( 4.248408730893249441, 6.358192987158595599, 14.59104375018031519 ) ) ;
#9759 = CARTESIAN_POINT ( 'NONE',  ( 4.276731815070940357, 10.32494394706615815, -1.822297250286802450 ) ) ;
#9760 = CARTESIAN_POINT ( 'NONE',  ( 0.000000000000000000, 0.000000000000000000, 0.000000000000000000 ) ) ;
#9761 = LINE ( 'NONE', #18018, #14398 ) ;
#9762 = DIRECTION ( 'NONE',  ( -1.000000000000000000, 0.000000000000000000, 0.000000000000000000 ) ) ;
#9763 = VERTEX_POINT ( 'NONE', #18041 ) ;
#9764 = CYLINDRICAL_SURFACE ( 'NONE', #12943, 2.649999999999993694 ) ;
#9765 = CARTESIAN_POINT ( 'NONE',  ( -12.72792205982779912, 12.72792206288790950, 10.34917500018031333 ) ) ;
#9766 = CARTESIAN_POINT ( 'NONE',  ( 30.00000000000000000, -39.99999999999999289, -49.90000000000000568 ) ) ;
#9767 = B_SPLINE_CURVE_WITH_KNOTS ( 'NONE', 3,
 ( #20643, #18758, #7728, #10703, #18865, #1055 ),
 .UNSPECIFIED., .F., .F.,
 ( 4, 2, 4 ),
 ( 0.002336974151641576809, 0.003500975885716453226, 0.004664977619791330077 ),
 .UNSPECIFIED. ) ;
#9768 = VERTEX_POINT ( 'NONE', #9979 ) ;
#9769 = EDGE_CURVE ( 'NONE', #3604, #2557, #15022, .T. ) ;
#9770 = CARTESIAN_POINT ( 'NONE',  ( 30.00000000000000000, 4.299168419249259188, -90.00000000000001421 ) ) ;
#9771 = ORIENTED_EDGE ( 'NONE', *, *, #4130, .F. ) ;
#9772 = DIRECTION ( 'NONE',  ( -0.000000000000000000, -0.000000000000000000, 1.000000000000000000 ) ) ;
#9773 = DIRECTION ( 'NONE',  ( 0.000000000000000000, 1.000000000000000000, 0.000000000000000000 ) ) ;
#9774 = ORIENTED_EDGE ( 'NONE', *, *, #1665, .F. ) ;
#9775 = ORIENTED_EDGE ( 'NONE', *, *, #18575, .T. ) ;
#9776 = CARTESIAN_POINT ( 'NONE',  ( 0.000000000000000000, 0.000000000000000000, -5.599999999999999645 ) ) ;
#9777 = EDGE_CURVE ( 'NONE', #10607, #12734, #2163, .T. ) ;
#9778 = DIRECTION ( 'NONE',  ( 1.000000000000000000, 0.000000000000000000, 0.000000000000000000 ) ) ;
#9779 = FACE_BOUND ( 'NONE', #19512, .T. ) ;
#9780 = VERTEX_POINT ( 'NONE', #7205 ) ;
#9781 = CARTESIAN_POINT ( 'NONE',  ( 1.491842754445842134, -7.500000000179339210, 11.86051875018031332 ) ) ;
#9782 = EDGE_CURVE ( 'NONE', #10885, #788, #7580, .T. ) ;
#9783 = FACE_BOUND ( 'NONE', #19182, .T. ) ;
#9784 = LINE ( 'NONE', #8190, #2179 ) ;
#9785 = DIRECTION ( 'NONE',  ( 1.000000000000000000, 0.000000000000000000, 0.000000000000000000 ) ) ;
#9786 = ORIENTED_EDGE ( 'NONE', *, *, #20878, .T. ) ;
#9787 = DIRECTION ( 'NONE',  ( 1.000000000000000000, 0.000000000000000000, 0.000000000000000000 ) ) ;
#9788 = CARTESIAN_POINT ( 'NONE',  ( 19.99999999999999645, -38.69327817041812523, 52.53819777490620169 ) ) ;
#9789 = CARTESIAN_POINT ( 'NONE',  ( 19.99999999999999645, -1.971042061627920727, -64.80882494896108881 ) ) ;
#9790 = ORIENTED_EDGE ( 'NONE', *, *, #15195, .T. ) ;
#9791 = FACE_OUTER_BOUND ( 'NONE', #9664, .T. ) ;
#9792 = ORIENTED_EDGE ( 'NONE', *, *, #11741, .T. ) ;
#9793 = DIRECTION ( 'NONE',  ( -0.000000000000000000, -0.000000000000000000, -1.000000000000000000 ) ) ;
#9794 = VERTEX_POINT ( 'NONE', #15381 ) ;
#9795 = CARTESIAN_POINT ( 'NONE',  ( 40.00000000000000711, -122.3205080756887639, 80.28096411455982206 ) ) ;
#9796 = DIRECTION ( 'NONE',  ( 0.000000000000000000, -0.6310879443260433153, -0.7757112907044274586 ) ) ;
#9797 = CARTESIAN_POINT ( 'NONE',  ( 9.474249098604511587, 6.330490856366296271, 25.03401600064742993 ) ) ;
#9798 = EDGE_CURVE ( 'NONE', #5332, #4217, #864, .T. ) ;
#9799 = ORIENTED_EDGE ( 'NONE', *, *, #11497, .F. ) ;
#9800 = DIRECTION ( 'NONE',  ( -1.000000000000000000, 0.000000000000000000, 0.000000000000000000 ) ) ;
#9801 = ADVANCED_FACE ( 'NONE', ( #13578 ), #8794, .F. ) ;
#9802 = CARTESIAN_POINT ( 'NONE',  ( -9.850000000000012079, 0.000000000000000000, 43.00000000000000000 ) ) ;
#9803 = ORIENTED_EDGE ( 'NONE', *, *, #19952, .F. ) ;
#9804 = CARTESIAN_POINT ( 'NONE',  ( 7.500000000000002665, -9.015933403756338579E-10, -27.90119999981969556 ) ) ;
#9805 = LINE ( 'NONE', #10018, #5797 ) ;
#9806 = CARTESIAN_POINT ( 'NONE',  ( -12.50000000000000533, 0.000000000000000000, -43.00000000000000000 ) ) ;
#9807 = CYLINDRICAL_SURFACE ( 'NONE', #17504, 2.649999999999999467 ) ;
#9808 = AXIS2_PLACEMENT_3D ( 'NONE', #6721, #3648, #11604 ) ;
#9809 = ORIENTED_EDGE ( 'NONE', *, *, #8885, .F. ) ;
#9810 = CARTESIAN_POINT ( 'NONE',  ( 19.99999999999999645, -42.42902769288568976, 49.02903636734183124 ) ) ;
#9811 = VERTEX_POINT ( 'NONE', #11989 ) ;
#9812 = DIRECTION ( 'NONE',  ( -0.000000000000000000, -0.000000000000000000, -1.000000000000000000 ) ) ;
#9813 = DIRECTION ( 'NONE',  ( 0.000000000000000000, -0.4999999999999993339, 0.8660254037844390407 ) ) ;
#9814 = CARTESIAN_POINT ( 'NONE',  ( 6.929096494179683319, 2.870125741905213079, -3.375362499819685613 ) ) ;
#9815 = TOROIDAL_SURFACE ( 'NONE', #20648, 11.17999999999999439, 0.3200000000000012834 ) ;
#9816 = EDGE_LOOP ( 'NONE', ( #5935, #20859, #6373, #3332 ) ) ;
#9817 = DIRECTION ( 'NONE',  ( 1.000000000000000000, 0.000000000000000000, 0.000000000000000000 ) ) ;
#9818 = FACE_OUTER_BOUND ( 'NONE', #386, .T. ) ;
#9819 = CARTESIAN_POINT ( 'NONE',  ( 6.250000000000203393, 10.82531754730537266, -51.00000000000001421 ) ) ;
#9820 = CARTESIAN_POINT ( 'NONE',  ( 18.00000000000000355, -2.163824016901520597E-09, -4.966449999819690042 ) ) ;
#9821 = ORIENTED_EDGE ( 'NONE', *, *, #15598, .F. ) ;
#9822 = VECTOR ( 'NONE', #2905, 1000.000000000000000 ) ;
#9823 = CARTESIAN_POINT ( 'NONE',  ( -1.491842754445841690, 7.500000000179340987, 7.148018750180309411 ) ) ;
#9824 = FACE_OUTER_BOUND ( 'NONE', #8681, .T. ) ;
#9825 = CARTESIAN_POINT ( 'NONE',  ( 14.79893867758296544, -1.779016607511491977E-09, 0.6972080815190739855 ) ) ;
#9826 = FACE_OUTER_BOUND ( 'NONE', #1290, .T. ) ;
#9827 = TOROIDAL_SURFACE ( 'NONE', #12210, 4.000000000000000000, 0.2500000000000000000 ) ;
#9828 = EDGE_CURVE ( 'NONE', #10009, #10694, #18083, .T. ) ;
#9829 = ORIENTED_EDGE ( 'NONE', *, *, #10645, .T. ) ;
#9830 = CARTESIAN_POINT ( 'NONE',  ( 19.99999999999999645, -45.48683723007244595, 46.78012013466202035 ) ) ;
#9831 = CARTESIAN_POINT ( 'NONE',  ( 5.303300859536635770, 5.303300858261589923, 24.31057500018031803 ) ) ;
#9832 = CARTESIAN_POINT ( 'NONE',  ( 41.00037741435939154, -14.03198441848082467, 74.23899123100075315 ) ) ;
#9833 = ORIENTED_EDGE ( 'NONE', *, *, #11702, .F. ) ;
#9834 = FACE_OUTER_BOUND ( 'NONE', #18271, .T. ) ;
#9835 = ORIENTED_EDGE ( 'NONE', *, *, #7636, .T. ) ;
#9836 = CARTESIAN_POINT ( 'NONE',  ( 6.232799999999996565, 0.000000000000000000, 0.000000000000000000 ) ) ;
#9837 = CARTESIAN_POINT ( 'NONE',  ( 0.000000000000000000, 0.000000000000000000, 81.99999999999998579 ) ) ;
#9838 = AXIS2_PLACEMENT_3D ( 'NONE', #6929, #11810, #18273 ) ;
#9839 = ORIENTED_EDGE ( 'NONE', *, *, #17993, .T. ) ;
#9840 = EDGE_CURVE ( 'NONE', #17007, #7589, #1834, .T. ) ;
#9841 = ORIENTED_EDGE ( 'NONE', *, *, #12625, .F. ) ;
#9842 = CARTESIAN_POINT ( 'NONE',  ( 46.19699674809955781, -7.457365076151437400, 79.04478793936081615 ) ) ;
#9843 = EDGE_CURVE ( 'NONE', #11409, #12885, #2137, .T. ) ;
#9844 = FACE_OUTER_BOUND ( 'NONE', #12976, .T. ) ;
#9845 = FILL_AREA_STYLE ('',( #103 ) ) ;
#9846 = CARTESIAN_POINT ( 'NONE',  ( 0.000000000000000000, 62.46228066917814203, -18.86519267363391350 ) ) ;
#9847 = B_SPLINE_CURVE_WITH_KNOTS ( 'NONE', 3,
 ( #3695, #2119, #4206, #8575, #2629, #9499 ),
 .UNSPECIFIED., .F., .F.,
 ( 4, 2, 4 ),
 ( 0.002336974151641520864, 0.003500975885716454961, 0.004664977619791389057 ),
 .UNSPECIFIED. ) ;
#9848 = CARTESIAN_POINT ( 'NONE',  ( 4.000000000000003553, -1.933795701539622103, -0.2488376576623028413 ) ) ;
#9849 = CARTESIAN_POINT ( 'NONE',  ( -2.870125743571144028, -6.929096493489630859, 19.00901250018031519 ) ) ;
#9850 = CARTESIAN_POINT ( 'NONE',  ( -11.17563879704981922, 2.222972771497742972, -4.473078500286804093 ) ) ;
#9851 = DIRECTION ( 'NONE',  ( -1.000000000000000000, 0.000000000000000000, 0.000000000000000000 ) ) ;
#9852 = CYLINDRICAL_SURFACE ( 'NONE', #2578, 27.60000000002759890 ) ;
#9853 = EDGE_CURVE ( 'NONE', #125, #8080, #17066, .T. ) ;
#9854 = CIRCLE ( 'NONE', #10188, 17.50000000000000355 ) ;
#9855 = ORIENTED_EDGE ( 'NONE', *, *, #2600, .F. ) ;
#9856 = FACE_OUTER_BOUND ( 'NONE', #17380, .T. ) ;
#9857 = ADVANCED_FACE ( 'NONE', ( #10299 ), #17079, .F. ) ;
#9858 = CARTESIAN_POINT ( 'NONE',  ( -10.19618095047498052, 15.25966317163203101, 10.64370625018031191 ) ) ;
#9859 = DIRECTION ( 'NONE',  ( 0.000000000000000000, 0.2697967711570248839, -0.9629172873477991335 ) ) ;
#9860 = VECTOR ( 'NONE', #16539, 1000.000000000000000 ) ;
#9861 = ORIENTED_EDGE ( 'NONE', *, *, #3985, .F. ) ;
#9862 = CYLINDRICAL_SURFACE ( 'NONE', #119, 72.00000000007199219 ) ;
#9863 = ORIENTED_EDGE ( 'NONE', *, *, #12214, .F. ) ;
#9864 = DIRECTION ( 'NONE',  ( 0.000000000000000000, 0.000000000000000000, 1.000000000000000000 ) ) ;
#9865 = CARTESIAN_POINT ( 'NONE',  ( 30.02347015119159224, -47.99982825264939379, 71.66797303202216085 ) ) ;
#9866 = EDGE_CURVE ( 'NONE', #11163, #6966, #16759, .T. ) ;
#9867 = EDGE_LOOP ( 'NONE', ( #8418, #4054, #5605, #20311 ) ) ;
#9868 = VECTOR ( 'NONE', #18895, 1000.000000000000000 ) ;
#9869 = EDGE_LOOP ( 'NONE', ( #5948, #4078, #6376, #17956, #19355, #1417, #19658, #15034, #3493, #9835, #13753, #3831, #19340, #18274, #14948, #11860, #15630, #16275, #18844, #6757, #13377, #8927, #19977, #14594, #6191, #18451, #5766, #20332, #5651, #16608, #7701, #4122, #9454, #4896, #10057, #923, #6314, #13032, #20925, #9786, #7431, #13932, #3723, #6833, #1129, #10400, #603, #14873, #10109, #13422, #11999, #11255, #12356, #7413, #39, #16456, #2679, #737, #16955, #18007, #11149, #5583, #17948, #1896, #7716, #20649, #16197, #2882, #3045, #4080, #985, #16428, #3283, #1335, #29, #8199, #15258, #15167, #11484, #15299, #2004, #15548, #15443, #1503, #11599, #1044, #13142, #4741, #2512, #16377, #14804, #11948, #20185, #1968, #5378, #2681, #12267, #2154, #12481, #7130, #18726, #14745, #12511, #4608, #10131, #20763, #9612, #17472, #17994, #13435, #6893, #13309, #15318, #13586, #4090, #9456, #12698, #19569, #13855, #20683, #15396, #1457, #20397, #2264, #4171, #20360, #20765, #18289, #11610, #19423, #8300, #17500, #1500, #17613, #18713, #6950, #14385, #19025, #8583, #708, #7310, #7804, #17200, #20872, #1388, #13220, #3418, #2569, #4419, #4872, #17415, #20930, #8293, #18997, #5033, #3423, #13061, #6093, #8546, #6730, #11397, #3679, #7980, #19360, #9502, #10821, #7410, #3195, #14892, #15917, #15138, #11501, #5434, #10085, #2550, #8960, #5668, #8659, #4785, #13321, #320, #484, #1826, #14106, #3956, #12043, #12213, #11192, #11386 ) ) ;
#9870 = CYLINDRICAL_SURFACE ( 'NONE', #1899, 72.00000000007199219 ) ;
#9871 =( NAMED_UNIT ( * ) PLANE_ANGLE_UNIT ( ) SI_UNIT ( $, .RADIAN. ) );
#9872 = CYLINDRICAL_SURFACE ( 'NONE', #20098, 27.60000000002759890 ) ;
#9873 = CARTESIAN_POINT ( 'NONE',  ( 19.99999999999999645, 0.000000000000000000, 0.000000000000000000 ) ) ;
#9874 = CIRCLE ( 'NONE', #12597, 2.041999999999999815 ) ;
#9875 = EDGE_CURVE ( 'NONE', #1717, #18188, #19766, .T. ) ;
#9876 = ORIENTED_EDGE ( 'NONE', *, *, #8584, .T. ) ;
#9877 = EDGE_CURVE ( 'NONE', #18360, #19491, #18662, .T. ) ;
#9878 = CARTESIAN_POINT ( 'NONE',  ( -4.248408729364575365, 6.358192988180014105, 6.558956250180312253 ) ) ;
#9879 = DIRECTION ( 'NONE',  ( 0.000000000000000000, -0.4999999999999993894, 0.8660254037844389297 ) ) ;
#9880 = AXIS2_PLACEMENT_3D ( 'NONE', #2399, #15436, #18618 ) ;
#9881 = DIRECTION ( 'NONE',  ( -1.000000000000000000, 0.000000000000000000, 0.000000000000000000 ) ) ;
#9882 = DIRECTION ( 'NONE',  ( -0.000000000000000000, -0.000000000000000000, 1.000000000000000000 ) ) ;
#9883 = VERTEX_POINT ( 'NONE', #4133 ) ;
#9884 = DIRECTION ( 'NONE',  ( -1.000000000000000000, 0.000000000000000000, -0.000000000000000000 ) ) ;
#9885 = EDGE_CURVE ( 'NONE', #11056, #9780, #7932, .T. ) ;
#9886 = ORIENTED_EDGE ( 'NONE', *, *, #4709, .F. ) ;
#9887 = CARTESIAN_POINT ( 'NONE',  ( -3.580422614997675002, -17.99999999956958163, 14.62973125018031517 ) ) ;
#9888 = DIRECTION ( 'NONE',  ( 1.000000000000000000, -0.000000000000000000, -0.000000000000000000 ) ) ;
#9889 = AXIS2_PLACEMENT_3D ( 'NONE', #5696, #17162, #4101 ) ;
#9890 = ORIENTED_EDGE ( 'NONE', *, *, #14826, .T. ) ;
#9891 = AXIS2_PLACEMENT_3D ( 'NONE', #4441, #15675, #10907 ) ;
#9892 = CARTESIAN_POINT ( 'NONE',  ( 7.500000000000000000, 9.184850993605147944E-16, 40.00000000000000000 ) ) ;
#9893 = ORIENTED_EDGE ( 'NONE', *, *, #16095, .F. ) ;
#9894 = CARTESIAN_POINT ( 'NONE',  ( 19.99999999999999645, 39.37110852956814000, 51.51683813304883586 ) ) ;
#9895 = CLOSED_SHELL ( 'NONE', ( #17327, #16546, #13892, #8827, #4590, #8733, #9350, #18946, #19651, #66, #19818, #17820, #13873, #5052, #14350, #15058, #8240, #3663, #698, #15, #15944, #8680, #16991, #13337, #7691, #11535, #2986, #6944, #16320, #14403 ) ) ;
#9896 = VECTOR ( 'NONE', #6245, 1000.000000000000000 ) ;
#9897 = ORIENTED_EDGE ( 'NONE', *, *, #13269, .T. ) ;
#9898 = DIRECTION ( 'NONE',  ( -1.000000000000000000, 0.000000000000000000, 0.000000000000000000 ) ) ;
#9899 = DIRECTION ( 'NONE',  ( 1.000000000000000000, -0.000000000000000000, 0.000000000000000000 ) ) ;
#9900 = CARTESIAN_POINT ( 'NONE',  ( 11.17563879758428769, 2.222972768810838939, 25.62307850064743420 ) ) ;
#9902 = EDGE_LOOP ( 'NONE', ( #664, #12951, #15968, #6449 ) ) ;
#9901 = VECTOR ( 'NONE', #192, 1000.000000000000000 ) ;
#9903 = DIRECTION ( 'NONE',  ( 1.000000000000000000, 0.000000000000000000, 0.000000000000000000 ) ) ;
#9904 = CARTESIAN_POINT ( 'NONE',  ( 0.000000000000000000, 0.000000000000000000, 0.000000000000000000 ) ) ;
#9905 = AXIS2_PLACEMENT_3D ( 'NONE', #713, #19588, #9940 ) ;
#9906 = ORIENTED_EDGE ( 'NONE', *, *, #19332, .F. ) ;
#9907 = FACE_OUTER_BOUND ( 'NONE', #14644, .T. ) ;
#9908 = VERTEX_POINT ( 'NONE', #5312 ) ;
#9909 = CARTESIAN_POINT ( 'NONE',  ( 3.580422610670020322, -18.00000000043041126, 15.94526875018031298 ) ) ;
#9910 = DIRECTION ( 'NONE',  ( 0.000000000000000000, 0.8878852184023763305, -0.4600650377311499839 ) ) ;
#9911 = CARTESIAN_POINT ( 'NONE',  ( 2.500000000000000000, -1.178949249685214307, 2.042000000000001592 ) ) ;
#9912 = AXIS2_PLACEMENT_3D ( 'NONE', #8314, #14495, #20932 ) ;
#9913 = ORIENTED_EDGE ( 'NONE', *, *, #3184, .T. ) ;
#9914 = DIRECTION ( 'NONE',  ( -1.000000000000000000, -0.000000000000000000, -0.000000000000000000 ) ) ;
#9915 = ORIENTED_EDGE ( 'NONE', *, *, #5715, .T. ) ;
#9916 = CIRCLE ( 'NONE', #11288, 2.649999999999988365 ) ;
#9917 = DIRECTION ( 'NONE',  ( 0.000000000000000000, 0.000000000000000000, 1.000000000000000000 ) ) ;
#9918 = ADVANCED_FACE ( 'NONE', ( #3813 ), #20136, .F. ) ;
#9919 = VERTEX_POINT ( 'NONE', #18568 ) ;
#9920 = DIRECTION ( 'NONE',  ( 0.5017436386064959564, -6.031582975246068435E-11, 0.8650163704334813408 ) ) ;
#9921 = FACE_OUTER_BOUND ( 'NONE', #15485, .T. ) ;
#9922 = CIRCLE ( 'NONE', #5860, 65.24900000006525147 ) ;
#9923 = CARTESIAN_POINT ( 'NONE',  ( -3.580422614997675890, -17.99999999956958519, -11.74066874981969555 ) ) ;
#9924 = ORIENTED_EDGE ( 'NONE', *, *, #8108, .F. ) ;
#9925 = CARTESIAN_POINT ( 'NONE',  ( -7.500000000000002665, 1.491842755816068955, 5.380831250087785733 ) ) ;
#9926 = AXIS2_PLACEMENT_3D ( 'NONE', #19010, #18805, #10756 ) ;
#9927 = DIRECTION ( 'NONE',  ( -1.000000000000000000, -0.000000000000000000, -0.000000000000000000 ) ) ;
#9928 = CIRCLE ( 'NONE', #6212, 72.00000000007199219 ) ;
#9929 = CARTESIAN_POINT ( 'NONE',  ( 12.54593441562639988, -8.382925371439625906, 1.580801831519075495 ) ) ;
#9930 = ORIENTED_EDGE ( 'NONE', *, *, #6690, .F. ) ;
#9931 =( REPRESENTATION_RELATIONSHIP ('NONE','NONE', #13739, #12383 ) REPRESENTATION_RELATIONSHIP_WITH_TRANSFORMATION ( #1023 )SHAPE_REPRESENTATION_RELATIONSHIP( ) );
#9932 = ADVANCED_FACE ( 'NONE', ( #13486 ), #2446, .T. ) ;
#9933 = ORIENTED_EDGE ( 'NONE', *, *, #3136, .T. ) ;
#9934 = DIRECTION ( 'NONE',  ( -1.000000000000000000, -0.000000000000000000, 0.000000000000000000 ) ) ;
#9935 = DIRECTION ( 'NONE',  ( 1.000000000000000000, 0.000000000000000000, 0.000000000000000000 ) ) ;
#9936 = CARTESIAN_POINT ( 'NONE',  ( 30.73276154958900719, -40.16863665929199811, 66.40168251036186575 ) ) ;
#9937 = AXIS2_PLACEMENT_3D ( 'NONE', #7881, #11271, #4911 ) ;
#9938 = ORIENTED_EDGE ( 'NONE', *, *, #1205, .F. ) ;
#9939 = CIRCLE ( 'NONE', #10279, 27.60000000002760245 ) ;
#9940 = DIRECTION ( 'NONE',  ( 0.000000000000000000, 0.000000000000000000, 1.000000000000000000 ) ) ;
#9941 = ORIENTED_EDGE ( 'NONE', *, *, #3453, .F. ) ;
#9942 = DIRECTION ( 'NONE',  ( -1.000000000000000000, 0.000000000000000000, 0.000000000000000000 ) ) ;
#9943 = DIRECTION ( 'NONE',  ( -1.000000000000000000, 0.000000000000000000, -0.000000000000000000 ) ) ;
#9944 = EDGE_CURVE ( 'NONE', #16972, #7685, #5406, .T. ) ;
#9945 = VERTEX_POINT ( 'NONE', #15171 ) ;
#9946 = VERTEX_POINT ( 'NONE', #4675 ) ;
#9947 = CARTESIAN_POINT ( 'NONE',  ( 2.500000000000000000, 2.357898499370431722, -2.818925648462311528E-15 ) ) ;
#9948 = AXIS2_PLACEMENT_3D ( 'NONE', #19829, #11877, #2563 ) ;
#9949 = CIRCLE ( 'NONE', #19768, 17.50000000000000355 ) ;
#9950 = CARTESIAN_POINT ( 'NONE',  ( -27.96694501150314593, -24.74873734152930993, -130.0000000000000000 ) ) ;
#9951 = CARTESIAN_POINT ( 'NONE',  ( -30.00000000000000000, -85.00000000000000000, -1.040949779275250179E-14 ) ) ;
#9952 = EDGE_CURVE ( 'NONE', #5576, #10231, #13677, .T. ) ;
#9953 = CARTESIAN_POINT ( 'NONE',  ( -52.00000000000000000, -39.99999999999999289, 5.000000000000000000 ) ) ;
#9954 = CARTESIAN_POINT ( 'NONE',  ( -5.303300858261589035, 5.303300859536635770, 21.95432500018031874 ) ) ;
#9955 = AXIS2_PLACEMENT_3D ( 'NONE', #19950, #7445, #13926 ) ;
#9956 = CARTESIAN_POINT ( 'NONE',  ( 7.902369976724389566, -7.902369978624323110, 10.54801524971320070 ) ) ;
#9957 = DIRECTION ( 'NONE',  ( 0.000000000000000000, 0.000000000000000000, -1.000000000000000000 ) ) ;
#9958 = CARTESIAN_POINT ( 'NONE',  ( 0.000000000000000000, -61.72688495901601158, -19.84591825364075746 ) ) ;
#9959 = AXIS2_PLACEMENT_3D ( 'NONE', #11046, #7860, #14341 ) ;
#9960 = EDGE_LOOP ( 'NONE', ( #7863, #815, #19162, #6104 ) ) ;
#9961 = CARTESIAN_POINT ( 'NONE',  ( 50.00000000000000000, -160.0000000000000000, 0.000000000000000000 ) ) ;
#9962 = CARTESIAN_POINT ( 'NONE',  ( 10.19618095047497874, -15.25966317163203279, 15.35620625018031404 ) ) ;
#9963 = DIRECTION ( 'NONE',  ( -1.000000000000000000, 0.000000000000000000, -0.000000000000000000 ) ) ;
#9964 = ORIENTED_EDGE ( 'NONE', *, *, #19342, .T. ) ;
#9965 = LINE ( 'NONE', #16429, #17052 ) ;
#9966 = ORIENTED_EDGE ( 'NONE', *, *, #210, .T. ) ;
#9967 = DIRECTION ( 'NONE',  ( -1.000000000000000000, 0.000000000000000000, 0.000000000000000000 ) ) ;
#9968 = CYLINDRICAL_SURFACE ( 'NONE', #8012, 10.85999999999999410 ) ;
#9969 = VERTEX_POINT ( 'NONE', #20464 ) ;
#9970 = EDGE_LOOP ( 'NONE', ( #2094, #8502, #3320, #2286 ) ) ;
#9971 = AXIS2_PLACEMENT_3D ( 'NONE', #9515, #11211, #4335 ) ;
#9972 = DIRECTION ( 'NONE',  ( 0.000000000000000000, 0.000000000000000000, 1.000000000000000000 ) ) ;
#9973 = EDGE_CURVE ( 'NONE', #2396, #9250, #13303, .T. ) ;
#9974 = FILL_AREA_STYLE ('',( #11874 ) ) ;
#9975 = LINE ( 'NONE', #16146, #13358 ) ;
#9976 = EDGE_CURVE ( 'NONE', #17187, #8604, #8888, .T. ) ;
#9977 = VECTOR ( 'NONE', #1560, 1000.000000000000000 ) ;
#9978 = ADVANCED_FACE ( 'NONE', ( #15800 ), #20345, .T. ) ;
#9979 = CARTESIAN_POINT ( 'NONE',  ( 18.00000000000000000, 0.000000000000000000, -90.00000000000000000 ) ) ;
#9980 = B_SPLINE_CURVE_WITH_KNOTS ( 'NONE', 3,
 ( #13860, #4212, #20425, #2636, #10886, #18848, #7486, #9193, #15653, #12487, #2833, #13969, #20307, #15762, #7602, #4089, #18741, #10688, #7276, #5909, #18950, #4324, #17149, #9301, #7169, #18529, #13651, #10793, #8867, #20100, #12158, #829, #8982, #18625, #5577, #2724, #12058, #3990, #17038, #2526, #14397, #9618, #1675, #14506, #9718, #12586, #6326, #19257, #12813, #17887, #1470, #11203, #19159, #10992, #4636, #20841, #9413, #1265 ),
 .UNSPECIFIED., .F., .F.,
 ( 4, 2, 2, 2, 2, 2, 2, 2, 2, 2, 2, 2, 2, 2, 2, 2, 2, 2, 2, 2, 2, 2, 2, 2, 2, 2, 2, 2, 4 ),
 ( 6.992893892674702526E-18, 0.004580336630963589492, 0.009160673261927172045, 0.01030575741966808373, 0.01145084157740899541, 0.01374100989289079623, 0.01603117820837259705, 0.01717626236611349486, 0.01832134652385439266, 0.02290168315481797695, 0.02519185147029977603, 0.02633693562804066690, 0.02748201978578156124, 0.03206235641674509695, 0.03320744057448597047, 0.03435252473222685093, 0.03664269304770861185, 0.03893286136319037971, 0.04122302967867213369, 0.04580336630963566247, 0.04809353462511742339, 0.05038370294059917737, 0.05267387125608093829, 0.05496403957156269227, 0.05954437620252620716, 0.06183454451800795421, 0.06412471283348972206, 0.06870504946445318839, 0.07328538609541666859 ),
 .UNSPECIFIED. ) ;
#9981 = VERTEX_POINT ( 'NONE', #6049 ) ;
#9982 = CARTESIAN_POINT ( 'NONE',  ( 6.929096494179676213, 2.870125741905210415, 18.63473750018031083 ) ) ;
#9983 = DIRECTION ( 'NONE',  ( -0.000000000000000000, -0.000000000000000000, 1.000000000000000000 ) ) ;
#9984 = EDGE_CURVE ( 'NONE', #3302, #1227, #1399, .T. ) ;
#9985 = DIRECTION ( 'NONE',  ( -1.000000000000000000, 0.000000000000000000, -0.000000000000000000 ) ) ;
#9986 = DIRECTION ( 'NONE',  ( 0.000000000000000000, 1.000000000000000000, -8.673617379884034239E-17 ) ) ;
#9987 = FACE_OUTER_BOUND ( 'NONE', #15422, .T. ) ;
#9988 = EDGE_LOOP ( 'NONE', ( #2531, #12582 ) ) ;
#9989 = DIRECTION ( 'NONE',  ( 0.000000000000000000, -0.7812527682501556603, 0.6242147964454771714 ) ) ;
#9990 = ORIENTED_EDGE ( 'NONE', *, *, #7252, .T. ) ;
#9991 = CARTESIAN_POINT ( 'NONE',  ( 19.99999999999999645, -62.46228066917775834, -18.86519267363519958 ) ) ;
#9992 = DIRECTION ( 'NONE',  ( -1.000000000000000000, 0.000000000000000000, 0.000000000000000000 ) ) ;
#9993 = ORIENTED_EDGE ( 'NONE', *, *, #4160, .F. ) ;
#9994 = CYLINDRICAL_SURFACE ( 'NONE', #15670, 2.649999999999999467 ) ;
#9995 = ORIENTED_EDGE ( 'NONE', *, *, #12086, .T. ) ;
#9996 = CIRCLE ( 'NONE', #9677, 0.06721999999999977993 ) ;
#9997 = PRODUCT_DEFINITION_SHAPE ( 'NONE', 'NONE',  #15841 ) ;
#9998 = DIRECTION ( 'NONE',  ( 0.000000000000000000, -0.3984010898462486683, 0.9172113015054499385 ) ) ;
#9999 = DIRECTION ( 'NONE',  ( -1.000000000000000000, -0.000000000000000000, -0.000000000000000000 ) ) ;
#10000 = VERTEX_POINT ( 'NONE', #20775 ) ;
#10001 = ADVANCED_FACE ( 'NONE', ( #18780 ), #4154, .T. ) ;
#10002 = DIRECTION ( 'NONE',  ( 0.000000000000000000, 0.000000000000000000, -1.000000000000000000 ) ) ;
#10003 = DIRECTION ( 'NONE',  ( 1.000000000000000000, 0.000000000000000000, 0.000000000000000000 ) ) ;
#10004 = ADVANCED_FACE ( 'NONE', ( #20665 ), #7422, .T. ) ;
#10005 = AXIS2_PLACEMENT_3D ( 'NONE', #16033, #4376, #20684 ) ;
#10006 = ADVANCED_FACE ( 'NONE', ( #4569 ), #1192, .F. ) ;
#10007 = DIRECTION ( 'NONE',  ( 1.000000000000000000, 0.000000000000000000, 0.000000000000000000 ) ) ;
#10008 = CARTESIAN_POINT ( 'NONE',  ( 7.902369976724399336, -7.902369978624331104, 17.67073475064742993 ) ) ;
#10009 = VERTEX_POINT ( 'NONE', #17401 ) ;
#10010 = CIRCLE ( 'NONE', #6292, 27.60000000002759890 ) ;
#10012 = EDGE_CURVE ( 'NONE', #3008, #5939, #16630, .T. ) ;
#10011 = CARTESIAN_POINT ( 'NONE',  ( 0.000000000000000000, 0.000000000000000000, 68.00000000000000000 ) ) ;
#10013 = EDGE_CURVE ( 'NONE', #3647, #14496, #7883, .T. ) ;
#10014 = DIRECTION ( 'NONE',  ( 0.000000000000000000, 0.000000000000000000, 1.000000000000000000 ) ) ;
#10015 = EDGE_LOOP ( 'NONE', ( #1786, #1156, #7025, #5744 ) ) ;
#10016 = CARTESIAN_POINT ( 'NONE',  ( 50.00000000000000000, -97.49621075554985339, -111.6458212409894486 ) ) ;
#10017 = ORIENTED_EDGE ( 'NONE', *, *, #6087, .F. ) ;
#10018 = CARTESIAN_POINT ( 'NONE',  ( 50.00000000000000000, -124.9999999999999858, -90.00000000000001421 ) ) ;
#10019 = FACE_OUTER_BOUND ( 'NONE', #8983, .T. ) ;
#10020 = LINE ( 'NONE', #16488, #12761 ) ;
#10021 = STYLED_ITEM ( 'NONE', ( #4223 ), #15250 ) ;
#10022 = ORIENTED_EDGE ( 'NONE', *, *, #19330, .F. ) ;
#10023 = VECTOR ( 'NONE', #11778, 1000.000000000000000 ) ;
#10024 = DIRECTION ( 'NONE',  ( 0.000000000000000000, 0.000000000000000000, -1.000000000000000000 ) ) ;
#10025 = B_SPLINE_CURVE_WITH_KNOTS ( 'NONE', 3,
 ( #20661, #7633, #17287, #14114, #9331, #2761, #2667, #14216, #10919, #9227, #1394, #4672, #12627, #4565, #16004, #20568, #6045, #20874, #19088, #12518 ),
 .UNSPECIFIED., .F., .F.,
 ( 4, 2, 2, 2, 2, 2, 2, 2, 2, 4 ),
 ( 0.01071967184985863145, 0.01211474467708338262, 0.01350981750430813380, 0.01629996315875761187, 0.01909010881320709341, 0.02188025446765657148, 0.02467040012210604955, 0.02606547294933077297, 0.02746054577655549292, 0.03304083708545443171 ),
 .UNSPECIFIED. ) ;
#10026 = VERTEX_POINT ( 'NONE', #9336 ) ;
#10027 = DIRECTION ( 'NONE',  ( 0.000000000000000000, -1.040834085586084454E-15, 1.000000000000000000 ) ) ;
#10028 = EDGE_CURVE ( 'NONE', #17230, #14903, #9129, .T. ) ;
#10029 = CIRCLE ( 'NONE', #14764, 65.24900000006526568 ) ;
#10030 = AXIS2_PLACEMENT_3D ( 'NONE', #18082, #6826, #13205 ) ;
#10031 = CARTESIAN_POINT ( 'NONE',  ( -4.248408730893249441, -6.358192987158596488, -18.39645624981969263 ) ) ;
#10032 = VERTEX_POINT ( 'NONE', #17292 ) ;
#10033 = CARTESIAN_POINT ( 'NONE',  ( 0.000000000000000000, 0.000000000000000000, -43.00000000000000000 ) ) ;
#10034 = AXIS2_PLACEMENT_3D ( 'NONE', #20589, #6064, #12538 ) ;
#10035 = CARTESIAN_POINT ( 'NONE',  ( 0.000000000000000000, 8.857208570070804754, -71.45313048675076573 ) ) ;
#10036 = PRODUCT_CONTEXT ( 'NONE', #2486, 'mechanical' ) ;
#10037 = CARTESIAN_POINT ( 'NONE',  ( -1.779019326032424922E-09, -14.79893867758297610, 8.671541918841546348 ) ) ;
#10038 = EDGE_LOOP ( 'NONE', ( #4789, #17332, #15592 ) ) ;
#10039 = CIRCLE ( 'NONE', #7667, 2.649999999999988365 ) ;
#10040 = CARTESIAN_POINT ( 'NONE',  ( 5.303300859536631329, 5.303300858261585482, 8.620675000180307634 ) ) ;
#10041 = ORIENTED_EDGE ( 'NONE', *, *, #19081, .F. ) ;
#10042 = FACE_BOUND ( 'NONE', #2309, .T. ) ;
#10043 = AXIS2_PLACEMENT_3D ( 'NONE', #12292, #12615, #18767 ) ;
#10044 = CARTESIAN_POINT ( 'NONE',  ( 5.663308646854338768, -13.67243654778934747, -6.960604418480926370 ) ) ;
#10045 = EDGE_CURVE ( 'NONE', #20820, #14202, #7747, .T. ) ;
#10046 =( GEOMETRIC_REPRESENTATION_CONTEXT ( 3 ) GLOBAL_UNCERTAINTY_ASSIGNED_CONTEXT ( ( #12171 ) ) GLOBAL_UNIT_ASSIGNED_CONTEXT ( ( #234, #19927, #19618 ) ) REPRESENTATION_CONTEXT ( 'NONE', 'WORKASPACE' ) );
#10047 = DIRECTION ( 'NONE',  ( 0.000000000000000000, 3.469446951953615175E-16, 1.000000000000000000 ) ) ;
#10048 = ORIENTED_EDGE ( 'NONE', *, *, #10045, .F. ) ;
#10049 = CARTESIAN_POINT ( 'NONE',  ( 38.55309439416022599, -121.4058261247164268, 86.08339649466212506 ) ) ;
#10050 = CARTESIAN_POINT ( 'NONE',  ( 44.24299768761039786, -125.5422689251970638, -83.10177353372741038 ) ) ;
#10051 = ORIENTED_EDGE ( 'NONE', *, *, #13888, .F. ) ;
#10052 = CARTESIAN_POINT ( 'NONE',  ( -2.870125743571144028, -6.929096493489630859, 9.584012500180316252 ) ) ;
#10053 = EDGE_LOOP ( 'NONE', ( #10820, #8131, #15815, #1549 ) ) ;
#10054 = CARTESIAN_POINT ( 'NONE',  ( -4.000000000000000000, 0.000000000000000000, 0.000000000000000000 ) ) ;
#10055 = CARTESIAN_POINT ( 'NONE',  ( 2.163825119083639120E-09, 17.99999999999999645, 9.622700000180310909 ) ) ;
#10056 = VECTOR ( 'NONE', #7491, 1000.000000000000000 ) ;
#10057 = ORIENTED_EDGE ( 'NONE', *, *, #7803, .T. ) ;
#10058 = ORIENTED_EDGE ( 'NONE', *, *, #6765, .F. ) ;
#10059 = DIRECTION ( 'NONE',  ( 0.000000000000000000, -0.9422609221188237294, 0.3348796121709770590 ) ) ;
#10060 = VECTOR ( 'NONE', #8325, 1000.000000000000000 ) ;
#10061 = AXIS2_PLACEMENT_3D ( 'NONE', #7620, #4231, #6033 ) ;
#10062 = DIRECTION ( 'NONE',  ( 1.000000000000000000, 0.000000000000000000, 0.000000000000000000 ) ) ;
#10063 = LINE ( 'NONE', #19799, #5144 ) ;
#10064 = DIRECTION ( 'NONE',  ( 0.000000000000000000, -0.3984010898462486683, 0.9172113015054499385 ) ) ;
#10065 = CARTESIAN_POINT ( 'NONE',  ( 0.000000000000000000, 58.26603306961963824, 42.29739224042492651 ) ) ;
#10066 = CARTESIAN_POINT ( 'NONE',  ( -6.358192987158596488, 4.248408730893249441, 21.65979375018031661 ) ) ;
#10067 = APPLICATION_CONTEXT ( 'automotive_design' ) ;
#10068 = AXIS2_PLACEMENT_3D ( 'NONE', #17492, #15477, #14314 ) ;
#10069 = CARTESIAN_POINT ( 'NONE',  ( 6.330490858644138186, 9.474249097082495297, 7.897233999713197505 ) ) ;
#10070 = EDGE_CURVE ( 'NONE', #15500, #15651, #7526, .T. ) ;
#10071 = AXIS2_PLACEMENT_3D ( 'NONE', #7028, #11801, #10002 ) ;
#10072 = CARTESIAN_POINT ( 'NONE',  ( 7.500000000000009770, -8.788009009181406898E-15, -12.21129999999768501 ) ) ;
#10073 = DIRECTION ( 'NONE',  ( 0.000000000000000000, 0.000000000000000000, 1.000000000000000000 ) ) ;
#10074 = AXIS2_PLACEMENT_3D ( 'NONE', #1378, #9426, #3056 ) ;
#10075 = VERTEX_POINT ( 'NONE', #18892 ) ;
#10076 = CARTESIAN_POINT ( 'NONE',  ( 0.000000000000000000, 35.35772184876955038, -54.34979580218157480 ) ) ;
#10077 = CARTESIAN_POINT ( 'NONE',  ( -18.00000000000000000, 2.163826221265758884E-09, 18.59605000018031262 ) ) ;
#10078 = FACE_OUTER_BOUND ( 'NONE', #7948, .T. ) ;
#10079 = ORIENTED_EDGE ( 'NONE', *, *, #8108, .T. ) ;
#10080 = DIRECTION ( 'NONE',  ( 0.000000000000000000, 0.000000000000000000, 1.000000000000000000 ) ) ;
#10081 = VERTEX_POINT ( 'NONE', #12742 ) ;
#10082 = LINE ( 'NONE', #228, #1074 ) ;
#10083 = CARTESIAN_POINT ( 'NONE',  ( -11.50000000000000000, 0.000000000000000000, -81.99999999999998579 ) ) ;
#10084 = ORIENTED_EDGE ( 'NONE', *, *, #14028, .F. ) ;
#10085 = ORIENTED_EDGE ( 'NONE', *, *, #649, .T. ) ;
#10086 = DIRECTION ( 'NONE',  ( 0.000000000000000000, 0.000000000000000000, 1.000000000000000000 ) ) ;
#10087 =( NAMED_UNIT ( * ) SI_UNIT ( $, .STERADIAN. ) SOLID_ANGLE_UNIT ( ) );
#10088 = ADVANCED_FACE ( 'NONE', ( #5943 ), #12417, .T. ) ;
#10089 = DIRECTION ( 'NONE',  ( 0.000000000000000000, 0.000000000000000000, -1.000000000000000000 ) ) ;
#10090 = DIRECTION ( 'NONE',  ( 0.000000000000000000, 0.000000000000000000, -1.000000000000000000 ) ) ;
#10091 = CARTESIAN_POINT ( 'NONE',  ( 7.499999999820660790, -1.491842756249031954, 10.09333125018031119 ) ) ;
#10092 = CARTESIAN_POINT ( 'NONE',  ( 33.75963133984988929, -116.7035671405861308, -82.37576306755489952 ) ) ;
#10093 = CARTESIAN_POINT ( 'NONE',  ( 0.000000000000000000, 5.051668046482832750E-16, -4.000000000000000000 ) ) ;
#10094 = LINE ( 'NONE', #1937, #13018 ) ;
#10095 = DIRECTION ( 'NONE',  ( -1.000000000000000000, -0.000000000000000000, -0.000000000000000000 ) ) ;
#10096 = MANIFOLD_SOLID_BREP ( 'Mirror1', #5562 ) ;
#10097 = EDGE_LOOP ( 'NONE', ( #4919, #3446, #7373, #14134 ) ) ;
#10098 = DIRECTION ( 'NONE',  ( -0.000000000000000000, 1.000000000000000000, 0.000000000000000000 ) ) ;
#10099 = ORIENTED_EDGE ( 'NONE', *, *, #9206, .T. ) ;
#10100 = CARTESIAN_POINT ( 'NONE',  ( 20.55500000000001748, 0.000000000000000000, 2.500000000000000888 ) ) ;
#10101 = DIRECTION ( 'NONE',  ( -0.000000000000000000, -0.000000000000000000, 1.000000000000000000 ) ) ;
#10102 = ORIENTED_EDGE ( 'NONE', *, *, #7665, .F. ) ;
#10103 = EDGE_CURVE ( 'NONE', #14918, #2494, #16185, .T. ) ;
#10104 = DIRECTION ( 'NONE',  ( 0.000000000000000000, 0.000000000000000000, -1.000000000000000000 ) ) ;
#10105 = ORIENTED_EDGE ( 'NONE', *, *, #3374, .T. ) ;
#10106 = LINE ( 'NONE', #9695, #5432 ) ;
#10107 = FACE_BOUND ( 'NONE', #12757, .T. ) ;
#10108 = EDGE_CURVE ( 'NONE', #1061, #16392, #10546, .T. ) ;
#10109 = ORIENTED_EDGE ( 'NONE', *, *, #4432, .T. ) ;
#10110 = EDGE_CURVE ( 'NONE', #13160, #19902, #19498, .T. ) ;
#10111 = DIRECTION ( 'NONE',  ( 1.000000000000000000, 0.000000000000000000, 0.000000000000000000 ) ) ;
#10112 = CARTESIAN_POINT ( 'NONE',  ( 50.00000000000000000, 230.0000000000000000, -85.00000000000000000 ) ) ;
#10113 = ADVANCED_FACE ( 'NONE', ( #11350 ), #11541, .F. ) ;
#10114 = CARTESIAN_POINT ( 'NONE',  ( 0.000000000000000000, -64.44931368725528387, 10.18420179740584608 ) ) ;
#10115 = AXIS2_PLACEMENT_3D ( 'NONE', #10733, #4253, #12526 ) ;
#10116 = CARTESIAN_POINT ( 'NONE',  ( 11.17563879704982632, -2.222972771497745637, 7.362141000647429934 ) ) ;
#10117 = EDGE_LOOP ( 'NONE', ( #15179, #18953, #3354, #2062 ) ) ;
#10118 = CARTESIAN_POINT ( 'NONE',  ( -4.000000000000000000, -2.309401076758531346, -5.242734410091827613 ) ) ;
#10119 = CARTESIAN_POINT ( 'NONE',  ( 17.00000000000000000, 0.000000000000000000, 0.000000000000000000 ) ) ;
#10120 = ORIENTED_EDGE ( 'NONE', *, *, #7421, .F. ) ;
#10121 = CYLINDRICAL_SURFACE ( 'NONE', #12869, 72.00000000007199219 ) ;
#10122 = EDGE_CURVE ( 'NONE', #10739, #18397, #1421, .T. ) ;
#10123 = ORIENTED_EDGE ( 'NONE', *, *, #2612, .T. ) ;
#10124 = CARTESIAN_POINT ( 'NONE',  ( -15.25966316918061771, 10.19618095414378622, 0.6296437501803129333 ) ) ;
#10125 = DIRECTION ( 'NONE',  ( 0.000000000000000000, 0.6310879443260539734, -0.7757112907044189098 ) ) ;
#10126 = DIRECTION ( 'NONE',  ( 1.000000000000000000, 0.000000000000000000, 0.000000000000000000 ) ) ;
#10127 = EDGE_CURVE ( 'NONE', #10560, #18447, #8503, .T. ) ;
#10128 = ORIENTED_EDGE ( 'NONE', *, *, #4792, .F. ) ;
#10129 = EDGE_CURVE ( 'NONE', #12459, #20061, #6848, .T. ) ;
#10130 = DIRECTION ( 'NONE',  ( 1.000000000000000000, 0.000000000000000000, 0.000000000000000000 ) ) ;
#10131 = ORIENTED_EDGE ( 'NONE', *, *, #16466, .T. ) ;
#10132 = DIRECTION ( 'NONE',  ( 1.000000000000000000, 1.836909530733573776E-16, 0.000000000000000000 ) ) ;
#10133 = EDGE_CURVE ( 'NONE', #1227, #14029, #1511, .T. ) ;
#10134 = ORIENTED_EDGE ( 'NONE', *, *, #3610, .T. ) ;
#10135 = CYLINDRICAL_SURFACE ( 'NONE', #12083, 27.60000000002760245 ) ;
#10136 = DIRECTION ( 'NONE',  ( 1.000000000000000000, 1.836909530733573776E-16, 0.000000000000000000 ) ) ;
#10137 = PRODUCT_CONTEXT ( 'NONE', #12520, 'mechanical' ) ;
#10138 = CARTESIAN_POINT ( 'NONE',  ( -14.79893867758297610, 1.779018419858781159E-09, 20.45279191884155168 ) ) ;
#10139 = VERTEX_POINT ( 'NONE', #107 ) ;
#10140 = DIRECTION ( 'NONE',  ( 0.000000000000000000, 0.000000000000000000, 1.000000000000000000 ) ) ;
#10141 = ADVANCED_FACE ( 'NONE', ( #17822 ), #8260, .F. ) ;
#10142 = CARTESIAN_POINT ( 'NONE',  ( 0.000000000000000000, 0.000000000000000000, -130.0000000000000000 ) ) ;
#10143 = ADVANCED_FACE ( 'NONE', ( #16222 ), #1706, .T. ) ;
#10144 = AXIS2_PLACEMENT_3D ( 'NONE', #7159, #10461, #3982 ) ;
#10145 = CARTESIAN_POINT ( 'NONE',  ( 6.888301784570727726, 16.62983158437509701, 19.63676250018031411 ) ) ;
#10146 = PLANE ( 'NONE',  #20349 ) ;
#10147 = VERTEX_POINT ( 'NONE', #18121 ) ;
#10148 = ADVANCED_FACE ( 'NONE', ( #9540 ), #3382, .T. ) ;
#10149 = DIRECTION ( 'NONE',  ( -0.000000000000000000, -0.000000000000000000, 1.000000000000000000 ) ) ;
#10150 = CARTESIAN_POINT ( 'NONE',  ( -2.870125741905210415, 6.929096494179677990, 16.27848750018030799 ) ) ;
#10151 = ORIENTED_EDGE ( 'NONE', *, *, #20429, .T. ) ;
#10152 = DIRECTION ( 'NONE',  ( 1.000000000000000000, 0.000000000000000000, 0.000000000000000000 ) ) ;
#10153 = ORIENTED_EDGE ( 'NONE', *, *, #18922, .T. ) ;
#10154 = DIRECTION ( 'NONE',  ( 0.000000000000000000, 0.000000000000000000, 1.000000000000000000 ) ) ;
#10155 = CARTESIAN_POINT ( 'NONE',  ( -12.72792205982779556, 12.72792206288790773, 8.444575000180309488 ) ) ;
#10156 = VERTEX_POINT ( 'NONE', #13151 ) ;
#10157 = ORIENTED_EDGE ( 'NONE', *, *, #17169, .F. ) ;
#10158 = CYLINDRICAL_SURFACE ( 'NONE', #8339, 27.60000000002760245 ) ;
#10159 = VECTOR ( 'NONE', #6588, 1000.000000000000000 ) ;
#10160 = CARTESIAN_POINT ( 'NONE',  ( 0.000000000000000000, 0.000000000000000000, 0.000000000000000000 ) ) ;
#10161 = DIRECTION ( 'NONE',  ( 0.000000000000000000, -1.000000000000000000, 0.000000000000000000 ) ) ;
#10162 =( NAMED_UNIT ( * ) SI_UNIT ( $, .STERADIAN. ) SOLID_ANGLE_UNIT ( ) );
#10163 = CARTESIAN_POINT ( 'NONE',  ( 10.19618095414378978, 15.25966316918061771, 21.83589375018031475 ) ) ;
#10164 = CARTESIAN_POINT ( 'NONE',  ( 7.499999999820668783, -1.491842756249033508, -2.491768749819687656 ) ) ;
#10165 = CARTESIAN_POINT ( 'NONE',  ( 10.32494394809438987, 4.276731812588564274, -19.49417225028681244 ) ) ;
#10166 = PRODUCT_DEFINITION_SHAPE ( 'NONE', 'NONE',  #20963 ) ;
#10167 = CARTESIAN_POINT ( 'NONE',  ( 30.00000000000000000, -85.00000000000000000, -1.040949779275250179E-14 ) ) ;
#10168 = CARTESIAN_POINT ( 'NONE',  ( 50.00000000000000000, -49.99999999999997868, 71.93747284969079203 ) ) ;
#10169 = ORIENTED_EDGE ( 'NONE', *, *, #18089, .F. ) ;
#10170 = FACE_OUTER_BOUND ( 'NONE', #11872, .T. ) ;
#10171 = AXIS2_PLACEMENT_3D ( 'NONE', #16571, #19866, #11602 ) ;
#10172 = CARTESIAN_POINT ( 'NONE',  ( 17.99999999956958163, -3.580422614997676334, 4.753081250180312800 ) ) ;
#10173 = DIRECTION ( 'NONE',  ( -1.000000000000000000, 0.000000000000000000, 0.000000000000000000 ) ) ;
#10174 = ORIENTED_EDGE ( 'NONE', *, *, #14410, .T. ) ;
#10175 = LINE ( 'NONE', #8379, #1777 ) ;
#10176 = VERTEX_POINT ( 'NONE', #19601 ) ;
#10177 = VECTOR ( 'NONE', #8708, 1000.000000000000000 ) ;
#10178 = CARTESIAN_POINT ( 'NONE',  ( 50.00000000000000000, 230.0000000000000000, 0.000000000000000000 ) ) ;
#10179 = DIRECTION ( 'NONE',  ( -0.000000000000000000, 0.000000000000000000, -1.000000000000000000 ) ) ;
#10180 = VERTEX_POINT ( 'NONE', #5074 ) ;
#10181 = VECTOR ( 'NONE', #7864, 1000.000000000000000 ) ;
#10182 = VERTEX_POINT ( 'NONE', #15358 ) ;
#10183 = FACE_OUTER_BOUND ( 'NONE', #14514, .T. ) ;
#10184 = EDGE_CURVE ( 'NONE', #4685, #12559, #4795, .T. ) ;
#10185 =( LENGTH_UNIT ( ) NAMED_UNIT ( * ) SI_UNIT ( .MILLI., .METRE. ) );
#10186 = DIRECTION ( 'NONE',  ( 0.000000000000000000, 0.000000000000000000, 1.000000000000000000 ) ) ;
#10187 = DIRECTION ( 'NONE',  ( 0.000000000000000000, 0.000000000000000000, 1.000000000000000000 ) ) ;
#10188 = AXIS2_PLACEMENT_3D ( 'NONE', #18731, #10878, #18943 ) ;
#10189 = CARTESIAN_POINT ( 'NONE',  ( -6.358192987158591158, 4.248408730893245000, -12.88010624981968810 ) ) ;
#10190 = CARTESIAN_POINT ( 'NONE',  ( 10.00000000000000178, -148.4917293642369600, 48.67032260359988527 ) ) ;
#10191 = CIRCLE ( 'NONE', #15262, 27.60000000002759890 ) ;
#10192 = DIRECTION ( 'NONE',  ( -0.000000000000000000, -0.000000000000000000, 1.000000000000000000 ) ) ;
#10193 = CARTESIAN_POINT ( 'NONE',  ( -6.165580000000000283, 0.000000000000000000, 10.79377999999999993 ) ) ;
#10194 = MANIFOLD_SOLID_BREP ( 'Mirror1', #7872 ) ;
#10195 = VERTEX_POINT ( 'NONE', #12074 ) ;
#10196 = CARTESIAN_POINT ( 'NONE',  ( 19.99999999999999645, 0.000000000000000000, 0.000000000000000000 ) ) ;
#10197 = EDGE_LOOP ( 'NONE', ( #5294, #13398, #8763, #16900 ) ) ;
#10198 = CARTESIAN_POINT ( 'NONE',  ( 3.580422614997668340, 17.99999999956958519, 9.917231250180313040 ) ) ;
#10199 = DIRECTION ( 'NONE',  ( 1.000000000000000000, 0.000000000000000000, 0.000000000000000000 ) ) ;
#10200 = VECTOR ( 'NONE', #5694, 1000.000000000000114 ) ;
#10201 = VERTEX_POINT ( 'NONE', #13776 ) ;
#10202 = CARTESIAN_POINT ( 'NONE',  ( 19.99999999999999645, -71.76067541710845887, -5.865617076725382795 ) ) ;
#10203 = VERTEX_POINT ( 'NONE', #14941 ) ;
#10204 = CARTESIAN_POINT ( 'NONE',  ( 62.49999999999999289, -40.00000000000000000, 5.000000000000000000 ) ) ;
#10205 = DIRECTION ( 'NONE',  ( 0.000000000000000000, 0.000000000000000000, -1.000000000000000000 ) ) ;
#10206 = ORIENTED_EDGE ( 'NONE', *, *, #11699, .F. ) ;
#10207 = COLOUR_RGB ( '', 0.31764706, 0.68627451, 0.89019608) ;
#10208 = CIRCLE ( 'NONE', #13272, 72.00000000007199219 ) ;
#10209 = EDGE_CURVE ( 'NONE', #15185, #5437, #14273, .T. ) ;
#10210 = CARTESIAN_POINT ( 'NONE',  ( 6.929096494179677990, 2.870125741905210859, -9.640262499819693076 ) ) ;
#10211 = CARTESIAN_POINT ( 'NONE',  ( -17.99999999999999645, 2.163826221265758470E-09, -11.58354999981969158 ) ) ;
#10212 = DIRECTION ( 'NONE',  ( -1.000000000000000000, -0.000000000000000000, -0.000000000000000000 ) ) ;
#10213 = DIRECTION ( 'NONE',  ( 0.000000000000000000, 0.000000000000000000, -1.000000000000000000 ) ) ;
#10214 = COLOUR_RGB ( '', 0.40784314, 0.44705882, 0.49803922) ;
#10215 = CARTESIAN_POINT ( 'NONE',  ( 10.32494394809439875, 4.276731812588567827, 15.90354725064743135 ) ) ;
#10216 = ADVANCED_FACE ( 'NONE', ( #18545 ), #841, .T. ) ;
#10217 = VERTEX_POINT ( 'NONE', #19803 ) ;
#10218 =( NAMED_UNIT ( * ) PLANE_ANGLE_UNIT ( ) SI_UNIT ( $, .RADIAN. ) );
#10219 = CARTESIAN_POINT ( 'NONE',  ( 0.000000000000000000, 0.000000000000000000, -40.00000000000000000 ) ) ;
#10220 = ORIENTED_EDGE ( 'NONE', *, *, #16708, .F. ) ;
#10221 = VECTOR ( 'NONE', #12031, 1000.000000000000000 ) ;
#10222 = CARTESIAN_POINT ( 'NONE',  ( 18.97564634267267181, -10.12806126886902014, -76.96678999104568675 ) ) ;
#10223 = AXIS2_PLACEMENT_3D ( 'NONE', #19708, #7083, #11973 ) ;
#10224 = ORIENTED_EDGE ( 'NONE', *, *, #8194, .F. ) ;
#10225 = CARTESIAN_POINT ( 'NONE',  ( -10.19618095414378622, -15.25966316918061416, -1.726606249819687910 ) ) ;
#10226 = CIRCLE ( 'NONE', #18349, 4.000000000000000000 ) ;
#10227 = DIRECTION ( 'NONE',  ( 1.000000000000000000, 1.836909530733573776E-16, 0.000000000000000000 ) ) ;
#10228 = CARTESIAN_POINT ( 'NONE',  ( 0.000000000000000000, -18.50424539729892714, 69.58155576219110117 ) ) ;
#10229 = EDGE_CURVE ( 'NONE', #4014, #9717, #16963, .T. ) ;
#10230 = ORIENTED_EDGE ( 'NONE', *, *, #9240, .T. ) ;
#10231 = VERTEX_POINT ( 'NONE', #3691 ) ;
#10232 = CARTESIAN_POINT ( 'NONE',  ( -22.96694501150314238, -24.74873734152930993, -120.0000000000000142 ) ) ;
#10233 = ORIENTED_EDGE ( 'NONE', *, *, #18143, .F. ) ;
#10234 = DIRECTION ( 'NONE',  ( -1.000000000000000000, -0.000000000000000000, 0.000000000000000000 ) ) ;
#10235 = AXIS2_PLACEMENT_3D ( 'NONE', #12596, #9727, #4644 ) ;
#10236 = AXIS2_PLACEMENT_3D ( 'NONE', #18499, #9934, #16402 ) ;
#10237 = CIRCLE ( 'NONE', #15991, 21.50000000000000000 ) ;
#10238 = CARTESIAN_POINT ( 'NONE',  ( 0.000000000000000000, 64.44931368725535492, -10.18420179740539844 ) ) ;
#10239 = CARTESIAN_POINT ( 'NONE',  ( 8.382925368423272516, -12.54593441764187745, 17.21294816884154955 ) ) ;
#10240 = EDGE_CURVE ( 'NONE', #3307, #10946, #16408, .T. ) ;
#10241 = ORIENTED_EDGE ( 'NONE', *, *, #5690, .F. ) ;
#10242 = ADVANCED_FACE ( 'NONE', ( #8774 ), #3789, .F. ) ;
#10243 = CARTESIAN_POINT ( 'NONE',  ( 19.99999999999999645, 43.56693332842786504, 48.57318520917521454 ) ) ;
#10244 = VERTEX_POINT ( 'NONE', #18225 ) ;
#10245 = AXIS2_PLACEMENT_3D ( 'NONE', #505, #20197, #6951 ) ;
#10246 = DIRECTION ( 'NONE',  ( -1.000000000000000000, 0.000000000000000000, -0.000000000000000000 ) ) ;
#10247 = CARTESIAN_POINT ( 'NONE',  ( 14.79893867758296544, -1.779016607511491977E-09, -18.15279191848092921 ) ) ;
#10248 = DIRECTION ( 'NONE',  ( 0.8660254037844371533, 0.5000000000000025535, 0.000000000000000000 ) ) ;
#10249 = EDGE_CURVE ( 'NONE', #6577, #5841, #11854, .T. ) ;
#10250 = ADVANCED_FACE ( 'NONE', ( #2215 ), #12172, .T. ) ;
#10251 = CIRCLE ( 'NONE', #18036, 27.60000000002759535 ) ;
#10252 = VECTOR ( 'NONE', #20179, 1000.000000000000000 ) ;
#10253 = EDGE_LOOP ( 'NONE', ( #15922, #3032, #6681, #16329 ) ) ;
#10254 = CARTESIAN_POINT ( 'NONE',  ( 40.00000000000000000, -122.3205080756887639, 86.97287527660684248 ) ) ;
#10255 = CARTESIAN_POINT ( 'NONE',  ( 19.99999999999999645, -64.79224928664389438, 25.14373648582931864 ) ) ;
#10256 = ORIENTED_EDGE ( 'NONE', *, *, #16869, .F. ) ;
#10257 = CARTESIAN_POINT ( 'NONE',  ( -4.248408730893249441, -6.358192987158596488, 9.878543750180313054 ) ) ;
#10258 = VERTEX_POINT ( 'NONE', #16623 ) ;
#10259 = DIRECTION ( 'NONE',  ( 0.000000000000000000, 0.000000000000000000, 1.000000000000000000 ) ) ;
#10260 = CARTESIAN_POINT ( 'NONE',  ( -17.99999999956958163, 3.580422614997673669, 7.560981250180310198 ) ) ;
#10261 = ORIENTED_EDGE ( 'NONE', *, *, #10532, .F. ) ;
#10262 = CIRCLE ( 'NONE', #20412, 4.000000000000000000 ) ;
#10263 = VERTEX_POINT ( 'NONE', #10065 ) ;
#10264 = CARTESIAN_POINT ( 'NONE',  ( 19.99999999999999645, -64.52323195238624010, -6.389157729493822657 ) ) ;
#10265 = VECTOR ( 'NONE', #17506, 1000.000000000000000 ) ;
#10266 = EDGE_CURVE ( 'NONE', #6177, #8249, #12709, .T. ) ;
#10267 = CARTESIAN_POINT ( 'NONE',  ( -31.75000000000000000, 10.85999999999999410, 0.000000000000000000 ) ) ;
#10268 = CARTESIAN_POINT ( 'NONE',  ( 6.250000000000054179, 10.82531754730546147, -43.00000000000000000 ) ) ;
#10269 = CARTESIAN_POINT ( 'NONE',  ( 16.62983158603122646, 6.888301780572504640, 22.71948750018031049 ) ) ;
#10270 = AXIS2_PLACEMENT_3D ( 'NONE', #10314, #8719, #16665 ) ;
#10271 = PRODUCT_DEFINITION_CONTEXT ( 'detailed design', #3167, 'design' ) ;
#10272 = EDGE_CURVE ( 'NONE', #6330, #6855, #13710, .T. ) ;
#10273 = CARTESIAN_POINT ( 'NONE',  ( -6.929096494179684207, -2.870125741905212635, -8.087862499819687301 ) ) ;
#10274 = CARTESIAN_POINT ( 'NONE',  ( 2.222972771497739419, 11.17563879704981922, -20.96682850028681244 ) ) ;
#10275 = EDGE_CURVE ( 'NONE', #4757, #2970, #18322, .T. ) ;
#10276 = AXIS2_PLACEMENT_3D ( 'NONE', #6394, #12875, #9686 ) ;
#10277 = FACE_OUTER_BOUND ( 'NONE', #8578, .T. ) ;
#10278 = DIRECTION ( 'NONE',  ( -1.000000000000000000, 0.000000000000000000, -0.000000000000000000 ) ) ;
#10279 = AXIS2_PLACEMENT_3D ( 'NONE', #6361, #8154, #20943 ) ;
#10280 = AXIS2_PLACEMENT_3D ( 'NONE', #14050, #12452, #4601 ) ;
#10281 = ORIENTED_EDGE ( 'NONE', *, *, #3208, .F. ) ;
#10282 = DIRECTION ( 'NONE',  ( 0.000000000000000000, 0.000000000000000000, -1.000000000000000000 ) ) ;
#10283 = CARTESIAN_POINT ( 'NONE',  ( -6.888301784570738384, -16.62983158437509346, -11.44613749981969164 ) ) ;
#10284 = DIRECTION ( 'NONE',  ( -0.000000000000000000, -0.000000000000000000, 1.000000000000000000 ) ) ;
#10285 = VECTOR ( 'NONE', #5538, 1000.000000000000000 ) ;
#10286 = ORIENTED_EDGE ( 'NONE', *, *, #15884, .T. ) ;
#10287 = CARTESIAN_POINT ( 'NONE',  ( 30.00000000000000000, -39.99999999999999289, 52.00000000000000000 ) ) ;
#10288 = ORIENTED_EDGE ( 'NONE', *, *, #20348, .F. ) ;
#10289 = AXIS2_PLACEMENT_3D ( 'NONE', #17442, #9384, #15845 ) ;
#10290 = DIRECTION ( 'NONE',  ( -1.000000000000000000, -0.000000000000000000, -0.000000000000000000 ) ) ;
#10291 = CARTESIAN_POINT ( 'NONE',  ( -15.15000000000000036, 0.000000000000000000, 169.0000000000000000 ) ) ;
#10292 = ORIENTED_EDGE ( 'NONE', *, *, #14776, .T. ) ;
#10293 = VERTEX_POINT ( 'NONE', #6409 ) ;
#10294 = CARTESIAN_POINT ( 'NONE',  ( 19.99999999999999645, -6.872116855662673274, -64.47358224882424338 ) ) ;
#10295 = ADVANCED_FACE ( 'NONE', ( #11189 ), #4826, .T. ) ;
#10296 = CIRCLE ( 'NONE', #2524, 72.00000000007199219 ) ;
#10297 =( NAMED_UNIT ( * ) SI_UNIT ( $, .STERADIAN. ) SOLID_ANGLE_UNIT ( ) );
#10298 = CARTESIAN_POINT ( 'NONE',  ( 3.599999999999913936, -10.82531754730554496, 46.00000000000000711 ) ) ;
#10299 = FACE_OUTER_BOUND ( 'NONE', #19689, .T. ) ;
#10300 = AXIS2_PLACEMENT_3D ( 'NONE', #245, #1736, #14662 ) ;
#10301 = AXIS2_PLACEMENT_3D ( 'NONE', #3934, #11888, #3721 ) ;
#10302 = CARTESIAN_POINT ( 'NONE',  ( 7.500000000000000888, -9.015933403756337545E-10, 0.3738000001803111205 ) ) ;
#10303 = CARTESIAN_POINT ( 'NONE',  ( 39.99999999999999289, -122.3205080756887639, -86.97287527660684248 ) ) ;
#10304 = SURFACE_STYLE_FILL_AREA ( #11994 ) ;
#10305 = LINE ( 'NONE', #10625, #7465 ) ;
#10306 = CARTESIAN_POINT ( 'NONE',  ( 30.00000000000000000, 4.299168419249259188, 84.99999999999997158 ) ) ;
#10307 = ORIENTED_EDGE ( 'NONE', *, *, #10672, .T. ) ;
#10308 = EDGE_CURVE ( 'NONE', #4931, #19553, #19246, .T. ) ;
#10309 = DIRECTION ( 'NONE',  ( -1.000000000000000000, -0.000000000000000000, -0.000000000000000000 ) ) ;
#10310 = EDGE_LOOP ( 'NONE', ( #12240, #13330, #1953, #345, #6125 ) ) ;
#10311 = CARTESIAN_POINT ( 'NONE',  ( -16.62983158603122291, -6.888301780572501087, 6.677387500180313573 ) ) ;
#10312 = CARTESIAN_POINT ( 'NONE',  ( 9.482998254698369323, -19.29932845388887586, 71.54974094241292448 ) ) ;
#10313 = ORIENTED_EDGE ( 'NONE', *, *, #3743, .F. ) ;
#10314 = CARTESIAN_POINT ( 'NONE',  ( 6.165579999999996730, 0.000000000000000000, 0.000000000000000000 ) ) ;
#10315 = VERTEX_POINT ( 'NONE', #12893 ) ;
#10316 = DIRECTION ( 'NONE',  ( 0.000000000000000000, 0.000000000000000000, 1.000000000000000000 ) ) ;
#10317 = CYLINDRICAL_SURFACE ( 'NONE', #263, 27.60000000002759535 ) ;
#10318 = ORIENTED_EDGE ( 'NONE', *, *, #13882, .F. ) ;
#10319 = COLOUR_RGB ( '', 0.08235294, 0.09019608, 0.10196078) ;
#10320 = DIRECTION ( 'NONE',  ( -1.000000000000000000, -0.000000000000000000, 0.000000000000000000 ) ) ;
#10321 = CARTESIAN_POINT ( 'NONE',  ( 6.888301780572505528, -16.62983158603121581, -14.52886249981968980 ) ) ;
#10322 = CARTESIAN_POINT ( 'NONE',  ( -4.000000000000000000, -0.3902508023145539462, 2.371692252312039717E-17 ) ) ;
#10323 = PRODUCT_DEFINITION_FORMATION_WITH_SPECIFIED_SOURCE ( 'ANY', '', #13215, .NOT_KNOWN. ) ;
#10324 = CARTESIAN_POINT ( 'NONE',  ( 6.330490856366294494, -9.474249098604513364, 8.540266000647427802 ) ) ;
#10325 = ORIENTED_EDGE ( 'NONE', *, *, #2090, .F. ) ;
#10326 = DIRECTION ( 'NONE',  ( -1.000000000000000000, 0.000000000000000000, 0.000000000000000000 ) ) ;
#10327 = EDGE_LOOP ( 'NONE', ( #11096, #18422, #908, #10787 ) ) ;
#10328 = CARTESIAN_POINT ( 'NONE',  ( 21.39608139526261255, -2.344611746178258294, -83.84634603192273516 ) ) ;
#10329 = PRESENTATION_LAYER_ASSIGNMENT (  '', '', ( #16758 ) ) ;
#10330 = EDGE_LOOP ( 'NONE', ( #16862, #5636 ) ) ;
#10331 = EDGE_CURVE ( 'NONE', #8637, #2521, #3871, .T. ) ;
#10332 = CARTESIAN_POINT ( 'NONE',  ( 12.72792205982779734, -12.72792206288791128, -3.788324999819688177 ) ) ;
#10333 = DIRECTION ( 'NONE',  ( 0.000000000000000000, 0.1361666490962466225, -0.9906859460363307557 ) ) ;
#10334 = DIRECTION ( 'NONE',  ( -1.000000000000000000, 0.000000000000000000, 0.000000000000000000 ) ) ;
#10335 = EDGE_LOOP ( 'NONE', ( #18981, #3276, #10760, #14169 ) ) ;
#10336 = DIRECTION ( 'NONE',  ( -1.000000000000000000, 0.000000000000000000, 0.000000000000000000 ) ) ;
#10337 = VERTEX_POINT ( 'NONE', #14584 ) ;
#10338 = CARTESIAN_POINT ( 'NONE',  ( 50.00000000000000000, 4.299168419249259188, -90.00000000000001421 ) ) ;
#10339 = EDGE_CURVE ( 'NONE', #5939, #3008, #4571, .T. ) ;
#10340 = ORIENTED_EDGE ( 'NONE', *, *, #14879, .F. ) ;
#10341 = DIRECTION ( 'NONE',  ( 0.000000000000000000, 0.000000000000000000, 1.000000000000000000 ) ) ;
#10342 = VECTOR ( 'NONE', #9813, 1000.000000000000000 ) ;
#10343 = EDGE_LOOP ( 'NONE', ( #2949, #12571, #20021, #14346 ) ) ;
#10344 = CARTESIAN_POINT ( 'NONE',  ( -30.00000000000000000, -85.00000000000000000, -9.000000000000005329 ) ) ;
#10345 = AXIS2_PLACEMENT_3D ( 'NONE', #17926, #4888, #4682 ) ;
#10346 = PRODUCT ( 'socket head cap screw_iso_ISO 4762 M5 x 12 - 12N', 'socket head cap screw_iso_ISO 4762 M5 x 12 - 12N', '', ( #1983 ) ) ;
#10347 = FACE_OUTER_BOUND ( 'NONE', #935, .T. ) ;
#10348 = CARTESIAN_POINT ( 'NONE',  ( 8.382925371439633011, 12.54593441562640876, 23.69263566884154670 ) ) ;
#10349 = ORIENTED_EDGE ( 'NONE', *, *, #8978, .T. ) ;
#10350 = DIRECTION ( 'NONE',  ( 1.000000000000000000, 0.000000000000000000, 0.000000000000000000 ) ) ;
#10351 = ORIENTED_EDGE ( 'NONE', *, *, #2089, .T. ) ;
#10352 = PLANE ( 'NONE',  #7428 ) ;
#10353 = CARTESIAN_POINT ( 'NONE',  ( -5.663308650141535949, -13.67243654642774686, -15.20747941848092921 ) ) ;
#10354 = AXIS2_PLACEMENT_3D ( 'NONE', #17939, #6689, #233 ) ;
#10355 = CARTESIAN_POINT ( 'NONE',  ( -6.999999999999993783, -10.52399999999999025, 1.288818291422673979E-15 ) ) ;
#10356 = CIRCLE ( 'NONE', #3249, 3.199999999999994404 ) ;
#10357 = AXIS2_PLACEMENT_3D ( 'NONE', #1866, #9713, #8320 ) ;
#10358 = ORIENTED_EDGE ( 'NONE', *, *, #11250, .F. ) ;
#10359 = CYLINDRICAL_SURFACE ( 'NONE', #14782, 72.00000000007199219 ) ;
#10360 = CARTESIAN_POINT ( 'NONE',  ( 1.040949779275250179E-14, -85.00000000000000000, 19.00000000000000000 ) ) ;
#10361 = VERTEX_POINT ( 'NONE', #11293 ) ;
#10362 = ADVANCED_FACE ( 'NONE', ( #4514, #20828 ), #4106, .F. ) ;
#10363 = DIRECTION ( 'NONE',  ( -1.000000000000000000, -0.000000000000000000, 0.000000000000000000 ) ) ;
#10364 = VERTEX_POINT ( 'NONE', #12800 ) ;
#10365 = PLANE ( 'NONE',  #17989 ) ;
#10366 = CARTESIAN_POINT ( 'NONE',  ( -10.19618095414378445, -15.25966316918061239, 15.21879375018031233 ) ) ;
#10367 = EDGE_CURVE ( 'NONE', #8060, #3623, #7702, .T. ) ;
#10368 = VERTEX_POINT ( 'NONE', #957 ) ;
#10369 = ORIENTED_EDGE ( 'NONE', *, *, #16238, .T. ) ;
#10370 = CYLINDRICAL_SURFACE ( 'NONE', #17848, 8.999999999999998224 ) ;
#10371 = AXIS2_PLACEMENT_3D ( 'NONE', #14837, #6172, #11346 ) ;
#10372 = VECTOR ( 'NONE', #3050, 1000.000000000000000 ) ;
#10373 = CYLINDRICAL_SURFACE ( 'NONE', #2265, 72.00000000007199219 ) ;
#10374 = CYLINDRICAL_SURFACE ( 'NONE', #18359, 21.50000000000000000 ) ;
#10375 = EDGE_CURVE ( 'NONE', #5100, #5928, #9399, .T. ) ;
#10376 = CARTESIAN_POINT ( 'NONE',  ( -10.00000000000000000, 0.000000000000000000, 0.000000000000000000 ) ) ;
#10377 = CIRCLE ( 'NONE', #5285, 8.999999999999994671 ) ;
#10378 = PRESENTATION_LAYER_ASSIGNMENT (  '', '', ( #19516 ) ) ;
#10379 = CARTESIAN_POINT ( 'NONE',  ( -5.303300858261589035, 5.303300859536635770, 3.104325000180315541 ) ) ;
#10380 = LINE ( 'NONE', #2322, #17195 ) ;
#10381 = CARTESIAN_POINT ( 'NONE',  ( 11.17563879758427525, 2.222972768810836719, -9.774641000286804271 ) ) ;
#10382 = AXIS2_PLACEMENT_3D ( 'NONE', #10397, #5501, #19922 ) ;
#10383 = DIRECTION ( 'NONE',  ( -1.000000000000000000, 0.000000000000000000, -0.000000000000000000 ) ) ;
#10384 = ADVANCED_FACE ( 'NONE', ( #14178 ), #7905, .T. ) ;
#10385 = CIRCLE ( 'NONE', #18855, 27.60000000002760245 ) ;
#10386 = ORIENTED_EDGE ( 'NONE', *, *, #7015, .T. ) ;
#10387 = DIRECTION ( 'NONE',  ( -1.000000000000000000, -0.000000000000000000, 0.000000000000000000 ) ) ;
#10388 = AXIS2_PLACEMENT_3D ( 'NONE', #11318, #1680, #14402 ) ;
#10389 = CARTESIAN_POINT ( 'NONE',  ( -10.19618095414378622, -15.25966316918061416, -1.726606249819687688 ) ) ;
#10390 = DIRECTION ( 'NONE',  ( 1.000000000000000000, 0.000000000000000000, 0.000000000000000000 ) ) ;
#10391 = EDGE_LOOP ( 'NONE', ( #17533, #657, #19086, #8491, #16583 ) ) ;
#10392 = EDGE_CURVE ( 'NONE', #16888, #18949, #20818, .T. ) ;
#10393 = FACE_OUTER_BOUND ( 'NONE', #11343, .T. ) ;
#10394 = AXIS2_PLACEMENT_3D ( 'NONE', #13965, #9298, #2941 ) ;
#10395 = VERTEX_POINT ( 'NONE', #20618 ) ;
#10396 = FACE_OUTER_BOUND ( 'NONE', #10327, .T. ) ;
#10397 = CARTESIAN_POINT ( 'NONE',  ( 19.99999999999999645, 51.81019761368321497, 38.98425606966075918 ) ) ;
#10398 = VECTOR ( 'NONE', #11302, 1000.000000000000000 ) ;
#10399 = EDGE_CURVE ( 'NONE', #7195, #10684, #2188, .T. ) ;
#10400 = ORIENTED_EDGE ( 'NONE', *, *, #976, .F. ) ;
#10401 = EDGE_LOOP ( 'NONE', ( #10918, #8726 ) ) ;
#10402 = DIRECTION ( 'NONE',  ( 0.000000000000000000, 0.000000000000000000, 1.000000000000000000 ) ) ;
#10403 = EDGE_CURVE ( 'NONE', #16910, #1886, #4517, .T. ) ;
#10404 =( NAMED_UNIT ( * ) SI_UNIT ( $, .STERADIAN. ) SOLID_ANGLE_UNIT ( ) );
#10405 = DIRECTION ( 'NONE',  ( 0.000000000000000000, 0.000000000000000000, -1.000000000000000000 ) ) ;
#10406 = DIRECTION ( 'NONE',  ( 0.000000000000000000, 0.000000000000000000, -1.000000000000000000 ) ) ;
#10407 = VECTOR ( 'NONE', #13987, 1000.000000000000000 ) ;
#10408 = CARTESIAN_POINT ( 'NONE',  ( 6.929096494179676213, 2.870125741905210415, -0.2152624998196898953 ) ) ;
#10409 = AXIS2_PLACEMENT_3D ( 'NONE', #13001, #2064, #6517 ) ;
#10410 = CARTESIAN_POINT ( 'NONE',  ( 30.88344783082026979, -110.8959383681548303, -79.30904931452684536 ) ) ;
#10411 = DIRECTION ( 'NONE',  ( 0.000000000000000000, 0.000000000000000000, -1.000000000000000000 ) ) ;
#10412 = FACE_OUTER_BOUND ( 'NONE', #13783, .T. ) ;
#10413 = CARTESIAN_POINT ( 'NONE',  ( -65.00002539999999840, 5.400000000000000355, 0.000000000000000000 ) ) ;
#10414 = EDGE_CURVE ( 'NONE', #3991, #16258, #13382, .T. ) ;
#10415 = EDGE_CURVE ( 'NONE', #15624, #5352, #8623, .T. ) ;
#10416 = VERTEX_POINT ( 'NONE', #16480 ) ;
#10417 = CARTESIAN_POINT ( 'NONE',  ( 6.358192988180019434, 4.248408729364581582, 5.755106250180313410 ) ) ;
#10418 = VERTEX_POINT ( 'NONE', #11809 ) ;
#10419 = CARTESIAN_POINT ( 'NONE',  ( -3.580422614997675002, -17.99999999956958163, 5.204731250180315349 ) ) ;
#10420 = CARTESIAN_POINT ( 'NONE',  ( 85.00002539999999840, 0.000000000000000000, 7.500000000000000000 ) ) ;
#10421 = CIRCLE ( 'NONE', #12451, 2.649999999999999467 ) ;
#10422 = VERTEX_POINT ( 'NONE', #18272 ) ;
#10423 = CARTESIAN_POINT ( 'NONE',  ( -24.99999999999999289, -160.0000000000000000, 53.99496054166690584 ) ) ;
#10424 = ORIENTED_EDGE ( 'NONE', *, *, #12746, .F. ) ;
#10425 = LINE ( 'NONE', #16886, #6452 ) ;
#10426 = CARTESIAN_POINT ( 'NONE',  ( 19.99999999999999645, -49.77519642623978058, -42.18840861821836796 ) ) ;
#10427 = VECTOR ( 'NONE', #12221, 1000.000000000000000 ) ;
#10428 = EDGE_CURVE ( 'NONE', #19634, #9123, #11674, .T. ) ;
#10429 = ORIENTED_EDGE ( 'NONE', *, *, #5993, .T. ) ;
#10430 = CARTESIAN_POINT ( 'NONE',  ( 9.999999999999998224, 29.55812890832068973, -65.65300461859658299 ) ) ;
#10431 = CARTESIAN_POINT ( 'NONE',  ( 16.62983158437509346, -6.888301784570737496, -6.281987499819692289 ) ) ;
#10432 = CARTESIAN_POINT ( 'NONE',  ( -30.00000000000000000, -85.00000000000000000, 79.99999999999998579 ) ) ;
#10433 = CARTESIAN_POINT ( 'NONE',  ( -7.500000000000002665, -4.022542205827308438E-17, 14.51130000000230602 ) ) ;
#10434 = CARTESIAN_POINT ( 'NONE',  ( 11.17563879704982632, -2.222972771497745637, 16.78714100064743420 ) ) ;
#10435 = ORIENTED_EDGE ( 'NONE', *, *, #5284, .T. ) ;
#10436 = CARTESIAN_POINT ( 'NONE',  ( 19.99999999999999645, 0.000000000000000000, 0.000000000000000000 ) ) ;
#10437 = FACE_OUTER_BOUND ( 'NONE', #18672, .T. ) ;
#10438 = VERTEX_POINT ( 'NONE', #5125 ) ;
#10439 = CARTESIAN_POINT ( 'NONE',  ( 20.23544477270225173, -7.290198706429629638, -79.18558687180571098 ) ) ;
#10440 = VERTEX_POINT ( 'NONE', #5240 ) ;
#10441 = CARTESIAN_POINT ( 'NONE',  ( -6.888301780572501976, 16.62983158603122291, 10.93823750018031404 ) ) ;
#10442 = DIRECTION ( 'NONE',  ( 0.000000000000000000, 0.000000000000000000, -1.000000000000000000 ) ) ;
#10443 = DIRECTION ( 'NONE',  ( 1.000000000000000000, 1.836909530733573776E-16, 0.000000000000000000 ) ) ;
#10444 = ORIENTED_EDGE ( 'NONE', *, *, #8925, .T. ) ;
#10445 = DIRECTION ( 'NONE',  ( 0.000000000000000000, 0.000000000000000000, -1.000000000000000000 ) ) ;
#10446 = ORIENTED_EDGE ( 'NONE', *, *, #10110, .T. ) ;
#10447 = DIRECTION ( 'NONE',  ( -0.5000000000000055511, -0.8660254037844354880, 0.000000000000000000 ) ) ;
#10448 = EDGE_LOOP ( 'NONE', ( #20141, #11591, #14445, #6860 ) ) ;
#10449 = CARTESIAN_POINT ( 'NONE',  ( 0.000000000000000000, 0.000000000000000000, 40.00000000000000000 ) ) ;
#10450 = MANIFOLD_SOLID_BREP ( 'RollersSimplified', #9895 ) ;
#10451 = EDGE_LOOP ( 'NONE', ( #20835, #19960 ) ) ;
#10452 = CARTESIAN_POINT ( 'NONE',  ( 9.999999999999998224, -70.29359119158496583, 15.58239511117263554 ) ) ;
#10453 = ADVANCED_FACE ( 'NONE', ( #3339 ), #8209, .T. ) ;
#10454 = EDGE_CURVE ( 'NONE', #964, #4388, #10882, .T. ) ;
#10455 = DIRECTION ( 'NONE',  ( 0.000000000000000000, -1.000000000000000000, 1.287488025362403787E-15 ) ) ;
#10456 = CONTEXT_DEPENDENT_SHAPE_REPRESENTATION ( #11706, #1059 ) ;
#10457 = CARTESIAN_POINT ( 'NONE',  ( -5.663308646854337880, 13.67243654778935991, 22.21997941884154315 ) ) ;
#10458 = ORIENTED_EDGE ( 'NONE', *, *, #16992, .F. ) ;
#10459 = DIRECTION ( 'NONE',  ( 0.000000000000000000, 0.000000000000000000, -1.000000000000000000 ) ) ;
#10460 = EDGE_LOOP ( 'NONE', ( #13477, #4806, #5806, #11847 ) ) ;
#10461 = DIRECTION ( 'NONE',  ( -1.000000000000000000, -0.000000000000000000, 0.000000000000000000 ) ) ;
#10462 = CARTESIAN_POINT ( 'NONE',  ( -18.00000000043040771, -3.580422610670021211, 16.39691875018031197 ) ) ;
#10463 = DIRECTION ( 'NONE',  ( -1.000000000000000000, -0.000000000000000000, -0.000000000000000000 ) ) ;
#10464 = VECTOR ( 'NONE', #318, 1000.000000000000114 ) ;
#10465 = ORIENTED_EDGE ( 'NONE', *, *, #6344, .T. ) ;
#10466 = DIRECTION ( 'NONE',  ( 1.000000000000000000, 0.000000000000000000, 0.000000000000000000 ) ) ;
#10467 = CARTESIAN_POINT ( 'NONE',  ( 5.303300859536631329, 5.303300858261585482, 18.04567500018031012 ) ) ;
#10468 = EDGE_CURVE ( 'NONE', #13280, #11798, #9658, .T. ) ;
#10469 = VERTEX_POINT ( 'NONE', #586 ) ;
#10470 = CARTESIAN_POINT ( 'NONE',  ( -24.99999999999999289, 31.35083268962912584, 6.892027480330899929E-14 ) ) ;
#10471 = ORIENTED_EDGE ( 'NONE', *, *, #16708, .T. ) ;
#10472 = DIRECTION ( 'NONE',  ( -0.000000000000000000, -0.000000000000000000, -1.000000000000000000 ) ) ;
#10473 = CARTESIAN_POINT ( 'NONE',  ( 6.888301784570727726, 16.62983158437509701, 10.21176250018031162 ) ) ;
#10474 = ORIENTED_EDGE ( 'NONE', *, *, #565, .T. ) ;
#10475 = ORIENTED_EDGE ( 'NONE', *, *, #20770, .F. ) ;
#10476 = DIRECTION ( 'NONE',  ( 0.000000000000000000, -1.000000000000000000, 0.000000000000000000 ) ) ;
#10477 = EDGE_CURVE ( 'NONE', #15053, #9908, #16089, .T. ) ;
#10478 = LINE ( 'NONE', #13458, #7687 ) ;
#10479 = CARTESIAN_POINT ( 'NONE',  ( 50.00000000000000000, -139.6410161513775563, -82.60203400177307742 ) ) ;
#10480 = CARTESIAN_POINT ( 'NONE',  ( -16.62983158437510411, 6.888301784570731279, 19.18511250018030978 ) ) ;
#10481 = UNCERTAINTY_MEASURE_WITH_UNIT (LENGTH_MEASURE( 1.000000000000000082E-05 ), #5837, 'distance_accuracy_value', 'NONE');
#10482 =( NAMED_UNIT ( * ) PLANE_ANGLE_UNIT ( ) SI_UNIT ( $, .RADIAN. ) );
#10483 = CARTESIAN_POINT ( 'NONE',  ( 4.248408730893249441, 6.358192987158595599, -4.258956249819687123 ) ) ;
#10484 = CARTESIAN_POINT ( 'NONE',  ( 0.000000000000000000, 0.000000000000000000, 0.000000000000000000 ) ) ;
#10485 = EDGE_CURVE ( 'NONE', #11708, #15181, #8615, .T. ) ;
#10486 = CARTESIAN_POINT ( 'NONE',  ( -9.474249098604506258, -6.330490856366290053, -15.07620350028680711 ) ) ;
#10487 = DIRECTION ( 'NONE',  ( 0.000000000000000000, 0.000000000000000000, -1.000000000000000000 ) ) ;
#10488 = ORIENTED_EDGE ( 'NONE', *, *, #3891, .F. ) ;
#10489 = DIRECTION ( 'NONE',  ( 1.000000000000000000, 1.836909530733573776E-16, 0.000000000000000000 ) ) ;
#10490 = CARTESIAN_POINT ( 'NONE',  ( -15.25966316918061771, 10.19618095414378622, -8.795356249819686667 ) ) ;
#10491 = DIRECTION ( 'NONE',  ( 0.000000000000000000, 0.000000000000000000, 1.000000000000000000 ) ) ;
#10492 = ORIENTED_EDGE ( 'NONE', *, *, #2981, .T. ) ;
#10493 = EDGE_CURVE ( 'NONE', #3309, #10217, #4903, .T. ) ;
#10494 = DIRECTION ( 'NONE',  ( -1.000000000000000000, -0.000000000000000000, -0.000000000000000000 ) ) ;
#10495 = VERTEX_POINT ( 'NONE', #266 ) ;
#10496 = CARTESIAN_POINT ( 'NONE',  ( -65.00002539999999840, 9.184850993605147944E-16, 7.500000000000000000 ) ) ;
#10497 = FACE_BOUND ( 'NONE', #14926, .T. ) ;
#10498 = VERTEX_POINT ( 'NONE', #6718 ) ;
#10499 = ORIENTED_EDGE ( 'NONE', *, *, #10568, .T. ) ;
#10500 = FACE_OUTER_BOUND ( 'NONE', #14878, .T. ) ;
#10501 = MECHANICAL_DESIGN_GEOMETRIC_PRESENTATION_REPRESENTATION (  '', ( #15229 ), #22 ) ;
#10502 = CARTESIAN_POINT ( 'NONE',  ( 19.99999999999999645, -51.43306257653114955, -40.15061736769617795 ) ) ;
#10503 = DIRECTION ( 'NONE',  ( 0.000000000000000000, 0.000000000000000000, -1.000000000000000000 ) ) ;
#10504 = ADVANCED_FACE ( 'NONE', ( #8413 ), #19646, .F. ) ;
#10505 = CARTESIAN_POINT ( 'NONE',  ( -1.491842756249031510, -7.499999999820660790, 3.024581250180311986 ) ) ;
#10506 = EDGE_CURVE ( 'NONE', #14556, #2235, #516, .T. ) ;
#10507 = CYLINDRICAL_SURFACE ( 'NONE', #13893, 2.649999999999998579 ) ;
#10508 = CARTESIAN_POINT ( 'NONE',  ( 50.00000000000000000, 230.0000000000000000, -84.99999999999998579 ) ) ;
#10509 = PLANE ( 'NONE',  #17636 ) ;
#10510 = DIRECTION ( 'NONE',  ( 1.000000000000000000, 0.000000000000000000, 0.000000000000000000 ) ) ;
#10511 = MANIFOLD_SOLID_BREP ( 'Keyway', #17445 ) ;
#10512 = ORIENTED_EDGE ( 'NONE', *, *, #9080, .T. ) ;
#10513 = FACE_OUTER_BOUND ( 'NONE', #4066, .T. ) ;
#10514 = EDGE_LOOP ( 'NONE', ( #3607, #13444, #18879 ) ) ;
#10515 = ADVANCED_FACE ( 'NONE', ( #5870 ), #8944, .T. ) ;
#10516 = CARTESIAN_POINT ( 'NONE',  ( -2.163827323447878234E-09, -18.00000000000000000, 4.910200000180314106 ) ) ;
#10517 = CARTESIAN_POINT ( 'NONE',  ( 9.140901424055382307, -19.46372757881361437, 71.47335990888086599 ) ) ;
#10518 = CIRCLE ( 'NONE', #7466, 27.60000000002759180 ) ;
#10519 = ORIENTED_EDGE ( 'NONE', *, *, #8846, .T. ) ;
#10520 = PRODUCT_DEFINITION ( 'UNKNOWN', '', #9314, #10271 ) ;
#10521 = DIRECTION ( 'NONE',  ( -1.000000000000000000, -0.000000000000000000, 0.000000000000000000 ) ) ;
#10522 = VERTEX_POINT ( 'NONE', #15410 ) ;
#10523 = CARTESIAN_POINT ( 'NONE',  ( 50.00000000000000000, -1.326995226329880762, -84.99999999999998579 ) ) ;
#10524 = FACE_BOUND ( 'NONE', #14845, .T. ) ;
#10525 = DIRECTION ( 'NONE',  ( -1.000000000000000000, 0.000000000000000000, 0.000000000000000000 ) ) ;
#10526 = VERTEX_POINT ( 'NONE', #5752 ) ;
#10527 = CARTESIAN_POINT ( 'NONE',  ( 19.99999999999999645, 58.44960523466241398, 28.06621538408611016 ) ) ;
#10528 = EDGE_CURVE ( 'NONE', #16884, #18441, #20135, .T. ) ;
#10529 = CARTESIAN_POINT ( 'NONE',  ( 0.000000000000000000, 65.23577793412344761, 1.313498510941937036 ) ) ;
#10530 = CARTESIAN_POINT ( 'NONE',  ( 16.62983158603121936, 6.888301780572501976, -16.88511249981969442 ) ) ;
#10531 = DIRECTION ( 'NONE',  ( 0.000000000000000000, 0.000000000000000000, 1.000000000000000000 ) ) ;
#10532 = EDGE_CURVE ( 'NONE', #15935, #7195, #2895, .T. ) ;
#10533 = DIRECTION ( 'NONE',  ( 0.000000000000000000, -1.000000000000000000, 1.287488025362403787E-15 ) ) ;
#10534 = AXIS2_PLACEMENT_3D ( 'NONE', #2553, #8786, #8588 ) ;
#10535 = CARTESIAN_POINT ( 'NONE',  ( 1.343451552857795926E-09, 11.17563879731705789, -4.713640249352573086 ) ) ;
#10536 = ORIENTED_EDGE ( 'NONE', *, *, #7927, .F. ) ;
#10537 = CARTESIAN_POINT ( 'NONE',  ( 0.000000000000000000, -58.44960523466222213, -28.06621538408651872 ) ) ;
#10538 = ADVANCED_FACE ( 'NONE', ( #677 ), #899, .T. ) ;
#10539 = DIRECTION ( 'NONE',  ( -0.000000000000000000, -0.000000000000000000, 1.000000000000000000 ) ) ;
#10540 = ORIENTED_EDGE ( 'NONE', *, *, #1711, .T. ) ;
#10541 = CARTESIAN_POINT ( 'NONE',  ( 2.601994274788645534, -21.34541601844983560, -70.64469287327101199 ) ) ;
#10542 = EDGE_LOOP ( 'NONE', ( #11686, #8149, #17202, #970 ) ) ;
#10543 = CARTESIAN_POINT ( 'NONE',  ( 3.580422614997668340, 17.99999999956958519, 2.396831250180312622 ) ) ;
#10544 = DIRECTION ( 'NONE',  ( -1.000000000000000000, 0.000000000000000000, 0.000000000000000000 ) ) ;
#10545 = CARTESIAN_POINT ( 'NONE',  ( -24.99999999999999289, -40.41646384503856382, 66.42520834682601105 ) ) ;
#10546 = CIRCLE ( 'NONE', #14946, 2.649999999999999467 ) ;
#10547 = ORIENTED_EDGE ( 'NONE', *, *, #14819, .T. ) ;
#10548 = AXIS2_PLACEMENT_3D ( 'NONE', #15646, #12578, #15863 ) ;
#10549 = CYLINDRICAL_SURFACE ( 'NONE', #14328, 27.60000000002760245 ) ;
#10550 = ORIENTED_EDGE ( 'NONE', *, *, #1205, .T. ) ;
#10551 = CARTESIAN_POINT ( 'NONE',  ( 9.015937996181842420E-10, 7.500000000000007994, 13.70745000018031590 ) ) ;
#10552 = VERTEX_POINT ( 'NONE', #5542 ) ;
#10553 = DIRECTION ( 'NONE',  ( -1.000000000000000000, -0.000000000000000000, -0.000000000000000000 ) ) ;
#10554 =( GEOMETRIC_REPRESENTATION_CONTEXT ( 3 ) GLOBAL_UNCERTAINTY_ASSIGNED_CONTEXT ( ( #10481 ) ) GLOBAL_UNIT_ASSIGNED_CONTEXT ( ( #5837, #10732, #17197 ) ) REPRESENTATION_CONTEXT ( 'NONE', 'WORKASPACE' ) );
#10555 = CARTESIAN_POINT ( 'NONE',  ( 0.000000000000000000, 36.59093685910629290, 62.00889726308042782 ) ) ;
#10556 = DIRECTION ( 'NONE',  ( 0.000000000000000000, 0.000000000000000000, 1.000000000000000000 ) ) ;
#10557 = CARTESIAN_POINT ( 'NONE',  ( -10.46442989202484242, 10.46442989454075700, -6.644083081158454362 ) ) ;
#10558 = VECTOR ( 'NONE', #3228, 1000.000000000000000 ) ;
#10560 = VERTEX_POINT ( 'NONE', #12019 ) ;
#10559 = AXIS2_PLACEMENT_3D ( 'NONE', #11460, #4995, #14742 ) ;
#10561 = CARTESIAN_POINT ( 'NONE',  ( 6.359999999999995879, 10.52400000000000091, 0.000000000000000000 ) ) ;
#10562 = VECTOR ( 'NONE', #19276, 1000.000000000000000 ) ;
#10563 = EDGE_LOOP ( 'NONE', ( #20893, #6186, #8397, #12273 ) ) ;
#10564 = CARTESIAN_POINT ( 'NONE',  ( -12.58049110815190730, -17.44827660000074232, 78.15203050255141193 ) ) ;
#10565 = CARTESIAN_POINT ( 'NONE',  ( -16.62983158437509701, 6.888301784570728614, 7.855512500180310553 ) ) ;
#10566 = CARTESIAN_POINT ( 'NONE',  ( -24.99999999999999289, -85.00000000000000000, -1.040949779275250179E-14 ) ) ;
#10567 = ORIENTED_EDGE ( 'NONE', *, *, #1173, .T. ) ;
#10568 = EDGE_CURVE ( 'NONE', #1127, #10422, #20383, .T. ) ;
#10569 = CARTESIAN_POINT ( 'NONE',  ( 19.99999999999999645, 31.17893654894306721, -57.31758819669140337 ) ) ;
#10570 = CARTESIAN_POINT ( 'NONE',  ( -25.39999999999999858, 9.184850993605147944E-16, -7.500000000000000000 ) ) ;
#10571 = EDGE_CURVE ( 'NONE', #13592, #2919, #17801, .T. ) ;
#10572 = ORIENTED_EDGE ( 'NONE', *, *, #13772, .T. ) ;
#10573 = AXIS2_PLACEMENT_3D ( 'NONE', #6970, #17628, #3101 ) ;
#10574 = CARTESIAN_POINT ( 'NONE',  ( -10.00000000000000000, 0.000000000000000000, 0.000000000000000000 ) ) ;
#10575 = AXIS2_PLACEMENT_3D ( 'NONE', #16425, #3905, #5188 ) ;
#10576 = EDGE_LOOP ( 'NONE', ( #20411, #20444, #3022, #11146 ) ) ;
#10577 = CARTESIAN_POINT ( 'NONE',  ( -9.015947181032828388E-10, -7.500000000000002665, 2.730050000180308523 ) ) ;
#10578 = CARTESIAN_POINT ( 'NONE',  ( -12.72792205982779556, 12.72792206288790773, -19.83042499981969087 ) ) ;
#10579 = ORIENTED_EDGE ( 'NONE', *, *, #2852, .F. ) ;
#10580 = CIRCLE ( 'NONE', #13292, 14.49999999999999467 ) ;
#10581 = EDGE_LOOP ( 'NONE', ( #3177, #7490 ) ) ;
#10582 = CARTESIAN_POINT ( 'NONE',  ( 6.250000000000054179, 10.82531754730546147, 46.00000000000000711 ) ) ;
#10583 = DIRECTION ( 'NONE',  ( -1.000000000000000000, -0.000000000000000000, 0.000000000000000000 ) ) ;
#10584 = DIRECTION ( 'NONE',  ( 0.000000000000000000, -0.6310879443260593025, 0.7757112907044144690 ) ) ;
#10585 = CARTESIAN_POINT ( 'NONE',  ( 0.000000000000000000, 64.80702306891096498, 7.581672767546657532 ) ) ;
#10586 = SURFACE_STYLE_USAGE ( .BOTH. , #3786 ) ;
#10587 = CIRCLE ( 'NONE', #11592, 2.649999999999994582 ) ;
#10588 = CARTESIAN_POINT ( 'NONE',  ( 12.72792205982779912, -12.72792206288791483, 15.06167500018031014 ) ) ;
#10589 = MANIFOLD_SOLID_BREP ( 'EndChamfer', #8967 ) ;
#10590 = DIRECTION ( 'NONE',  ( 1.000000000000000000, 0.000000000000000000, 0.000000000000000000 ) ) ;
#10591 = CARTESIAN_POINT ( 'NONE',  ( 6.929096494179683319, 2.870125741905213079, 6.049637500180313765 ) ) ;
#10592 = VECTOR ( 'NONE', #2507, 1000.000000000000000 ) ;
#10593 = CARTESIAN_POINT ( 'NONE',  ( -9.015947181032835626E-10, -7.500000000000007994, 18.41995000018031803 ) ) ;
#10594 = AXIS2_PLACEMENT_3D ( 'NONE', #14719, #18390, #8347 ) ;
#10595 = CARTESIAN_POINT ( 'NONE',  ( -11.17563879731704723, 1.343452237168308679E-09, -23.61760975028680321 ) ) ;
#10596 = AXIS2_PLACEMENT_3D ( 'NONE', #2982, #6147, #979 ) ;
#10597 = AXIS2_PLACEMENT_3D ( 'NONE', #8746, #692, #5557 ) ;
#10598 = FACE_BOUND ( 'NONE', #14067, .T. ) ;
#10599 = ORIENTED_EDGE ( 'NONE', *, *, #9163, .T. ) ;
#10600 = EDGE_CURVE ( 'NONE', #306, #2456, #14736, .T. ) ;
#10601 = DIRECTION ( 'NONE',  ( -0.000000000000000000, -0.000000000000000000, -1.000000000000000000 ) ) ;
#10602 = CARTESIAN_POINT ( 'NONE',  ( -15.25966316918061771, 10.19618095414378622, 0.6296437501803129333 ) ) ;
#10603 = FACE_OUTER_BOUND ( 'NONE', #259, .T. ) ;
#10604 = CIRCLE ( 'NONE', #11952, 2.649999999999999467 ) ;
#10605 = VERTEX_POINT ( 'NONE', #6390 ) ;
#10606 = FACE_OUTER_BOUND ( 'NONE', #18210, .T. ) ;
#10607 = VERTEX_POINT ( 'NONE', #11267 ) ;
#10608 = LINE ( 'NONE', #543, #19334 ) ;
#10609 = LINE ( 'NONE', #5401, #17490 ) ;
#10610 = ORIENTED_EDGE ( 'NONE', *, *, #5126, .T. ) ;
#10611 = VERTEX_POINT ( 'NONE', #9470 ) ;
#10612 = EDGE_CURVE ( 'NONE', #12045, #17518, #20485, .T. ) ;
#10613 = DIRECTION ( 'NONE',  ( 1.000000000000000000, 0.000000000000000000, 0.000000000000000000 ) ) ;
#10614 = TOROIDAL_SURFACE ( 'NONE', #1146, 11.17999999999999261, 0.3200000000000008393 ) ;
#10615 = ADVANCED_FACE ( 'NONE', ( #12448 ), #12870, .T. ) ;
#10616 = VECTOR ( 'NONE', #8299, 1000.000000000000000 ) ;
#10617 = SURFACE_STYLE_USAGE ( .BOTH. , #11987 ) ;
#10618 = CARTESIAN_POINT ( 'NONE',  ( -2.500000000000000444, 3.061616997868384127E-16, 3.469446951953614189E-15 ) ) ;
#10619 = DIRECTION ( 'NONE',  ( 1.000000000000000000, 0.000000000000000000, 0.000000000000000000 ) ) ;
#10620 = VECTOR ( 'NONE', #17749, 1000.000000000000000 ) ;
#10621 = AXIS2_PLACEMENT_3D ( 'NONE', #13127, #5150, #11326 ) ;
#10622 = CARTESIAN_POINT ( 'NONE',  ( -7.499999999820661678, 1.491842756249031288, -4.044168749819689879 ) ) ;
#10623 = FILL_AREA_STYLE_COLOUR ( '', #9190 ) ;
#10624 = DIRECTION ( 'NONE',  ( 0.000000000000000000, 0.000000000000000000, 1.000000000000000000 ) ) ;
#10625 = CARTESIAN_POINT ( 'NONE',  ( 30.00000000000000000, -85.00000000000000000, 79.99999999999998579 ) ) ;
#10626 = CARTESIAN_POINT ( 'NONE',  ( 0.000000000000000000, 0.000000000000000000, 126.0000000000000000 ) ) ;
#10627 = AXIS2_PLACEMENT_3D ( 'NONE', #1524, #16135, #1630 ) ;
#10628 = ORIENTED_EDGE ( 'NONE', *, *, #17268, .T. ) ;
#10629 = CARTESIAN_POINT ( 'NONE',  ( 19.99999999999999645, -28.84646472442495480, 58.52617768068423487 ) ) ;
#10630 = ORIENTED_EDGE ( 'NONE', *, *, #20239, .T. ) ;
#10631 = CARTESIAN_POINT ( 'NONE',  ( -3.580422610670018546, 18.00000000043041126, -0.09683124981968786738 ) ) ;
#10632 = CARTESIAN_POINT ( 'NONE',  ( -6.110423144575286791, -20.66992657861277038, 70.93137971084414062 ) ) ;
#10633 =( REPRESENTATION_RELATIONSHIP ('NONE','NONE', #13739, #2344 ) REPRESENTATION_RELATIONSHIP_WITH_TRANSFORMATION ( #7470 )SHAPE_REPRESENTATION_RELATIONSHIP( ) );
#10634 = ORIENTED_EDGE ( 'NONE', *, *, #15884, .F. ) ;
#10635 = CARTESIAN_POINT ( 'NONE',  ( 0.000000000000000000, 48.70996102988680576, 42.79495875147792106 ) ) ;
#10636 = VERTEX_POINT ( 'NONE', #20803 ) ;
#10637 = EDGE_CURVE ( 'NONE', #4894, #18535, #9996, .T. ) ;
#10638 = CYLINDRICAL_SURFACE ( 'NONE', #16277, 27.60000000002759890 ) ;
#10639 = PLANE ( 'NONE',  #7360 ) ;
#10640 = CARTESIAN_POINT ( 'NONE',  ( 0.000000000000000000, 0.000000000000000000, 43.00000000000000000 ) ) ;
#10641 = VERTEX_POINT ( 'NONE', #7877 ) ;
#10642 = DIRECTION ( 'NONE',  ( 0.000000000000000000, 0.000000000000000000, -1.000000000000000000 ) ) ;
#10643 = AXIS2_PLACEMENT_3D ( 'NONE', #15220, #20086, #10459 ) ;
#10644 = EDGE_CURVE ( 'NONE', #1747, #17144, #14415, .T. ) ;
#10645 = EDGE_CURVE ( 'NONE', #7485, #7828, #7673, .T. ) ;
#10646 = CARTESIAN_POINT ( 'NONE',  ( 3.599999999999909051, -10.82531754730554496, 126.0000000000000000 ) ) ;
#10647 = CARTESIAN_POINT ( 'NONE',  ( -15.25966316918061416, 10.19618095414378445, -10.69995624981968874 ) ) ;
#10648 = CARTESIAN_POINT ( 'NONE',  ( 2.500000000000000000, -1.178949249685218303, -2.041999999999998039 ) ) ;
#10649 = AXIS2_PLACEMENT_3D ( 'NONE', #14162, #19135, #7572 ) ;
#10650 = DIRECTION ( 'NONE',  ( -1.000000000000000000, 0.000000000000000000, 0.000000000000000000 ) ) ;
#10651 = EDGE_CURVE ( 'NONE', #9351, #16482, #6178, .T. ) ;
#10652 = CARTESIAN_POINT ( 'NONE',  ( -6.330490858644140850, -9.474249097082498849, -8.542546499352576816 ) ) ;
#10653 = ORIENTED_EDGE ( 'NONE', *, *, #4929, .T. ) ;
#10654 = DIRECTION ( 'NONE',  ( 0.000000000000000000, 0.000000000000000000, -1.000000000000000000 ) ) ;
#10655 = ORIENTED_EDGE ( 'NONE', *, *, #19776, .T. ) ;
#10656 = CIRCLE ( 'NONE', #2478, 27.60000000002759890 ) ;
#10657 = CARTESIAN_POINT ( 'NONE',  ( 2.985015299703236646, -21.29524168283703744, -70.66569055735612892 ) ) ;
#10658 = VERTEX_POINT ( 'NONE', #9571 ) ;
#10659 = CARTESIAN_POINT ( 'NONE',  ( -15.25966316918061771, 10.19618095414378622, -18.22035624981969093 ) ) ;
#10660 = DIRECTION ( 'NONE',  ( -1.000000000000000000, 0.000000000000000000, -0.000000000000000000 ) ) ;
#10661 = LINE ( 'NONE', #2178, #8343 ) ;
#10662 = ORIENTED_EDGE ( 'NONE', *, *, #2705, .T. ) ;
#10663 = EDGE_CURVE ( 'NONE', #10885, #7362, #14361, .T. ) ;
#10664 = CARTESIAN_POINT ( 'NONE',  ( 19.99999999999999645, 0.000000000000000000, 0.000000000000000000 ) ) ;
#10665 = VERTEX_POINT ( 'NONE', #20911 ) ;
#10666 = CIRCLE ( 'NONE', #12357, 20.00000000000000000 ) ;
#10667 = DIRECTION ( 'NONE',  ( -1.000000000000000000, 0.000000000000000000, 0.000000000000000000 ) ) ;
#10668 = ORIENTED_EDGE ( 'NONE', *, *, #7120, .F. ) ;
#10669 = EDGE_CURVE ( 'NONE', #12643, #12564, #13046, .T. ) ;
#10670 = EDGE_CURVE ( 'NONE', #17353, #6509, #4304, .T. ) ;
#10671 = DIRECTION ( 'NONE',  ( 1.000000000000000000, 0.000000000000000000, 0.000000000000000000 ) ) ;
#10672 = EDGE_CURVE ( 'NONE', #11249, #11867, #7563, .T. ) ;
#10673 = LINE ( 'NONE', #5672, #3461 ) ;
#10674 = ITEM_DEFINED_TRANSFORMATION ( 'NONE', 'NONE', #203,  #12461 ) ;
#10675 = CARTESIAN_POINT ( 'NONE',  ( -2.943691925285397470, 14.79893867793684059, -5.760489331158455961 ) ) ;
#10676 = VERTEX_POINT ( 'NONE', #4598 ) ;
#10677 = PLANE ( 'NONE',  #17707 ) ;
#10678 = VERTEX_POINT ( 'NONE', #4383 ) ;
#10679 = CARTESIAN_POINT ( 'NONE',  ( -17.90548703470696879, -11.90519517575888919, 81.89175300428205162 ) ) ;
#10680 = CARTESIAN_POINT ( 'NONE',  ( 10.19618095047497697, -15.25966317163202923, 13.45160625018031197 ) ) ;
#10681 = DIRECTION ( 'NONE',  ( -1.000000000000000000, -0.000000000000000000, -0.000000000000000000 ) ) ;
#10682 = LINE ( 'NONE', #13963, #551 ) ;
#10683 = EDGE_CURVE ( 'NONE', #17979, #3309, #17319, .T. ) ;
#10684 = VERTEX_POINT ( 'NONE', #2795 ) ;
#10685 = LINE ( 'NONE', #17354, #4980 ) ;
#10686 = DIRECTION ( 'NONE',  ( 0.000000000000000000, 0.000000000000000000, -1.000000000000000000 ) ) ;
#10687 = ORIENTED_EDGE ( 'NONE', *, *, #20764, .F. ) ;
#10688 = CARTESIAN_POINT ( 'NONE',  ( 15.22879382678786975, -17.29418148938178845, -78.22818066287017302 ) ) ;
#10689 = EDGE_LOOP ( 'NONE', ( #5027, #15214, #11790, #16228, #16214, #7884, #2803, #901 ) ) ;
#10690 = AXIS2_PLACEMENT_3D ( 'NONE', #20355, #9239, #9033 ) ;
#10691 = DIRECTION ( 'NONE',  ( -0.000000000000000000, -0.000000000000000000, 1.000000000000000000 ) ) ;
#10692 = CARTESIAN_POINT ( 'NONE',  ( -17.99999999999999645, 2.163826221265758470E-09, -21.00854999981969229 ) ) ;
#10693 = EDGE_CURVE ( 'NONE', #8981, #1332, #17434, .T. ) ;
#10694 = VERTEX_POINT ( 'NONE', #4488 ) ;
#10695 = VERTEX_POINT ( 'NONE', #10957 ) ;
#10696 = DIRECTION ( 'NONE',  ( -1.000000000000000000, 0.000000000000000000, -0.000000000000000000 ) ) ;
#10697 = DIRECTION ( 'NONE',  ( -1.000000000000000000, -0.000000000000000000, -0.000000000000000000 ) ) ;
#10698 = DIRECTION ( 'NONE',  ( 1.384478184788908018E-16, -1.611744734445712550E-26, -1.000000000000000000 ) ) ;
#10699 = LINE ( 'NONE', #5587, #6507 ) ;
#10700 = CARTESIAN_POINT ( 'NONE',  ( 17.99999999956958519, -3.580422614997676778, 14.17808125018031085 ) ) ;
#10701 = EDGE_CURVE ( 'NONE', #14496, #11746, #15834, .T. ) ;
#10702 = AXIS2_PLACEMENT_3D ( 'NONE', #9360, #4790, #19005 ) ;
#10703 = CARTESIAN_POINT ( 'NONE',  ( 3.344563996438205677, 2.687817229851463097, -0.1586754815284831532 ) ) ;
#10704 = VERTEX_POINT ( 'NONE', #17635 ) ;
#10705 = DIRECTION ( 'NONE',  ( -1.000000000000000000, 0.000000000000000000, 0.000000000000000000 ) ) ;
#10706 = AXIS2_PLACEMENT_3D ( 'NONE', #112, #16226, #18019 ) ;
#10707 = CARTESIAN_POINT ( 'NONE',  ( 11.17563879731704723, -1.343450868547281106E-09, -28.33010975028681244 ) ) ;
#10708 = PRODUCT_DEFINITION_SHAPE ( 'NONE', 'NONE',  #19582 ) ;
#10709 = CARTESIAN_POINT ( 'NONE',  ( 9.999999999999998224, 70.68211945903188109, 13.71269443944232336 ) ) ;
#10710 = ORIENTED_EDGE ( 'NONE', *, *, #6223, .F. ) ;
#10711 = DIRECTION ( 'NONE',  ( -1.000000000000000000, 0.000000000000000000, -0.000000000000000000 ) ) ;
#10712 = CARTESIAN_POINT ( 'NONE',  ( 6.888301784570728614, 16.62983158437510056, -16.15863749981969377 ) ) ;
#10713 = CARTESIAN_POINT ( 'NONE',  ( 19.99999999999999645, 0.000000000000000000, 0.000000000000000000 ) ) ;
#10714 = VERTEX_POINT ( 'NONE', #7773 ) ;
#10715 = FACE_OUTER_BOUND ( 'NONE', #3858, .T. ) ;
#10716 = ORIENTED_EDGE ( 'NONE', *, *, #10339, .F. ) ;
#10717 = DIRECTION ( 'NONE',  ( 1.000000000000000000, 0.000000000000000000, 0.000000000000000000 ) ) ;
#10718 = CYLINDRICAL_SURFACE ( 'NONE', #14460, 17.50000000000000355 ) ;
#10719 = VECTOR ( 'NONE', #7094, 1000.000000000000000 ) ;
#10720 = ORIENTED_EDGE ( 'NONE', *, *, #8962, .F. ) ;
#10721 = ORIENTED_EDGE ( 'NONE', *, *, #631, .T. ) ;
#10722 = DIRECTION ( 'NONE',  ( 0.000000000000000000, 0.000000000000000000, 1.000000000000000000 ) ) ;
#10723 = VECTOR ( 'NONE', #2718, 1000.000000000000114 ) ;
#10724 = AXIS2_PLACEMENT_3D ( 'NONE', #15699, #7532, #15493 ) ;
#10725 =( LENGTH_UNIT ( ) NAMED_UNIT ( * ) SI_UNIT ( .MILLI., .METRE. ) );
#10726 = LINE ( 'NONE', #2668, #10265 ) ;
#10727 = EDGE_CURVE ( 'NONE', #16131, #16334, #20693, .T. ) ;
#10728 = ADVANCED_FACE ( 'NONE', ( #1733 ), #17944, .T. ) ;
#10729 = AXIS2_PLACEMENT_3D ( 'NONE', #20682, #3097, #10746 ) ;
#10730 = DIRECTION ( 'NONE',  ( 1.000000000000000000, 0.000000000000000000, 0.000000000000000000 ) ) ;
#10731 = CARTESIAN_POINT ( 'NONE',  ( -4.248408729364575365, 6.358192988180014105, -21.71604374981968988 ) ) ;
#10732 =( NAMED_UNIT ( * ) PLANE_ANGLE_UNIT ( ) SI_UNIT ( $, .RADIAN. ) );
#10733 = CARTESIAN_POINT ( 'NONE',  ( 19.99999999999999645, 0.000000000000000000, 0.000000000000000000 ) ) ;
#10734 = CARTESIAN_POINT ( 'NONE',  ( 50.00000000000000000, -30.00000000000000711, 44.99999999999998579 ) ) ;
#10735 = AXIS2_PLACEMENT_3D ( 'NONE', #1975, #5741, #13919 ) ;
#10736 = ORIENTED_EDGE ( 'NONE', *, *, #18842, .T. ) ;
#10737 = STYLED_ITEM ( 'NONE', ( #447 ), #3656 ) ;
#10738 = CARTESIAN_POINT ( 'NONE',  ( 0.000000000000000000, 0.000000000000000000, -81.99999999999998579 ) ) ;
#10739 = VERTEX_POINT ( 'NONE', #6696 ) ;
#10740 = CARTESIAN_POINT ( 'NONE',  ( 15.25966317163202746, 10.19618095047498407, -7.754643749819687848 ) ) ;
#10741 = FACE_OUTER_BOUND ( 'NONE', #3887, .T. ) ;
#10742 = VERTEX_POINT ( 'NONE', #18045 ) ;
#10743 = CARTESIAN_POINT ( 'NONE',  ( 0.000000000000000000, -63.48283426024829623, -33.96954156735433372 ) ) ;
#10744 = ORIENTED_EDGE ( 'NONE', *, *, #10864, .T. ) ;
#10745 = FACE_OUTER_BOUND ( 'NONE', #4763, .T. ) ;
#10746 = DIRECTION ( 'NONE',  ( -1.648349939164583989E-16, 1.000000000000000000, 0.000000000000000000 ) ) ;
#10747 = CIRCLE ( 'NONE', #4988, 65.24900000006526568 ) ;
#10748 = ORIENTED_EDGE ( 'NONE', *, *, #17964, .T. ) ;
#10749 = CARTESIAN_POINT ( 'NONE',  ( 19.99999999999999645, 15.58726123847851142, 62.93731870009410301 ) ) ;
#10750 = AXIS2_PLACEMENT_3D ( 'NONE', #284, #1875, #11616 ) ;
#10751 = LINE ( 'NONE', #2475, #19853 ) ;
#10752 = CARTESIAN_POINT ( 'NONE',  ( 30.00000000000000000, -122.0000000000000000, 2.099999999999984102 ) ) ;
#10753 = CARTESIAN_POINT ( 'NONE',  ( 19.99999999999999645, -61.72688495901601158, -19.84591825364075746 ) ) ;
#10754 = VECTOR ( 'NONE', #6828, 1000.000000000000000 ) ;
#10755 = AXIS2_PLACEMENT_3D ( 'NONE', #6874, #15363, #7300 ) ;
#10756 = DIRECTION ( 'NONE',  ( 0.000000000000000000, -0.1361666490962539222, 0.9906859460363298675 ) ) ;
#10757 = EDGE_LOOP ( 'NONE', ( #9560, #8858, #639, #687, #4667, #18304 ) ) ;
#10758 = SURFACE_STYLE_FILL_AREA ( #17219 ) ;
#10759 = DIRECTION ( 'NONE',  ( -1.000000000000000000, 0.000000000000000000, 0.000000000000000000 ) ) ;
#10760 = ORIENTED_EDGE ( 'NONE', *, *, #9606, .T. ) ;
#10761 = CIRCLE ( 'NONE', #7715, 2.700000000000000622 ) ;
#10762 = FACE_OUTER_BOUND ( 'NONE', #18215, .T. ) ;
#10763 = DIRECTION ( 'NONE',  ( 1.000000000000000000, 0.000000000000000000, 0.000000000000000000 ) ) ;
#10764 = ADVANCED_FACE ( 'NONE', ( #14968 ), #14674, .F. ) ;
#10765 = ORIENTED_EDGE ( 'NONE', *, *, #11033, .T. ) ;
#10766 = CARTESIAN_POINT ( 'NONE',  ( -15.25966316918061771, 10.19618095414378622, -8.795356249819686667 ) ) ;
#10767 = DIRECTION ( 'NONE',  ( 1.000000000000000000, 0.000000000000000000, 0.000000000000000000 ) ) ;
#10768 = CARTESIAN_POINT ( 'NONE',  ( 1.318516776095788545, 3.857556137907071747, 2.454790609853964971E-15 ) ) ;
#10769 = ORIENTED_EDGE ( 'NONE', *, *, #1555, .F. ) ;
#10770 = CYLINDRICAL_SURFACE ( 'NONE', #8207, 65.24900000006525147 ) ;
#10771 = ORIENTED_EDGE ( 'NONE', *, *, #2103, .F. ) ;
#10772 = CARTESIAN_POINT ( 'NONE',  ( 2.500000000000000000, -1.178949249685213863, 2.042000000000002924 ) ) ;
#10773 = ORIENTED_EDGE ( 'NONE', *, *, #6891, .T. ) ;
#10774 = ADVANCED_FACE ( 'NONE', ( #20798 ), #1110, .T. ) ;
#10775 = CARTESIAN_POINT ( 'NONE',  ( 31.94921915542539637, -113.6563480467028029, 75.04517990444932707 ) ) ;
#10776 = DIRECTION ( 'NONE',  ( 1.000000000000000000, 0.000000000000000000, 0.000000000000000000 ) ) ;
#10777 = CARTESIAN_POINT ( 'NONE',  ( 12.54593441562640876, -8.382925371439629458, -2.226114331158456139 ) ) ;
#10778 = VERTEX_POINT ( 'NONE', #10752 ) ;
#10779 = CARTESIAN_POINT ( 'NONE',  ( 9.999999999999998224, -20.34307325858833337, 69.06634035770301239 ) ) ;
#10780 = ORIENTED_EDGE ( 'NONE', *, *, #18504, .F. ) ;
#10781 = CARTESIAN_POINT ( 'NONE',  ( -18.38761746031185496, -11.14595575959862295, 82.49318946023234389 ) ) ;
#10782 = EDGE_CURVE ( 'NONE', #7756, #12404, #9319, .T. ) ;
#10783 = CARTESIAN_POINT ( 'NONE',  ( 16.62983158603121936, 6.888301780572501976, 1.964887500180308777 ) ) ;
#10784 = EDGE_CURVE ( 'NONE', #1298, #9221, #10950, .T. ) ;
#10785 = DIRECTION ( 'NONE',  ( -1.000000000000000000, 0.000000000000000000, 0.000000000000000000 ) ) ;
#10786 = LINE ( 'NONE', #15539, #7993 ) ;
#10787 = ORIENTED_EDGE ( 'NONE', *, *, #10571, .T. ) ;
#10788 = ADVANCED_FACE ( 'NONE', ( #14039 ), #14241, .T. ) ;
#10789 = CYLINDRICAL_SURFACE ( 'NONE', #6991, 27.60000000002759890 ) ;
#10790 = LINE ( 'NONE', #20304, #3972 ) ;
#10791 = VECTOR ( 'NONE', #4463, 1000.000000000000000 ) ;
#10792 = ORIENTED_EDGE ( 'NONE', *, *, #16490, .T. ) ;
#10793 = CARTESIAN_POINT ( 'NONE',  ( 4.250247840617388917, -22.60715243308596101, -75.54244079978928994 ) ) ;
#10794 = CARTESIAN_POINT ( 'NONE',  ( 0.000000000000000000, 0.000000000000000000, -5.600000000000000533 ) ) ;
#10795 = CARTESIAN_POINT ( 'NONE',  ( -3.580422614997674557, -17.99999999956957808, -4.220268749819691578 ) ) ;
#10796 = ORIENTED_EDGE ( 'NONE', *, *, #3873, .F. ) ;
#10797 = FACE_OUTER_BOUND ( 'NONE', #13212, .T. ) ;
#10798 = FACE_OUTER_BOUND ( 'NONE', #17338, .T. ) ;
#10799 = CARTESIAN_POINT ( 'NONE',  ( 19.99999999999999645, 55.05624179292029652, -35.01774179823726740 ) ) ;
#10800 = DIRECTION ( 'NONE',  ( -1.000000000000000000, 0.000000000000000000, 0.000000000000000000 ) ) ;
#10801 = DIRECTION ( 'NONE',  ( 0.000000000000000000, 0.000000000000000000, 1.000000000000000000 ) ) ;
#10802 = EDGE_CURVE ( 'NONE', #16683, #9551, #4594, .T. ) ;
#10803 = CARTESIAN_POINT ( 'NONE',  ( 6.888301784570730391, 16.62983158437510411, 2.691362500180309425 ) ) ;
#10804 = EDGE_CURVE ( 'NONE', #4175, #13894, #13724, .T. ) ;
#10805 = CARTESIAN_POINT ( 'NONE',  ( 9.015937996181842420E-10, 7.500000000000007994, -14.56754999981968446 ) ) ;
#10806 = ORIENTED_EDGE ( 'NONE', *, *, #3284, .F. ) ;
#10807 = CARTESIAN_POINT ( 'NONE',  ( -4.248408730893249441, -6.358192987158596488, 19.30354375018031732 ) ) ;
#10808 = CARTESIAN_POINT ( 'NONE',  ( -5.663308650141535949, -13.67243654642774686, 13.06752058151907647 ) ) ;
#10809 = EDGE_CURVE ( 'NONE', #15954, #20245, #4248, .T. ) ;
#10810 = FACE_OUTER_BOUND ( 'NONE', #7189, .T. ) ;
#10811 = ORIENTED_EDGE ( 'NONE', *, *, #14519, .F. ) ;
#10812 = DIRECTION ( 'NONE',  ( 1.000000000000000000, 1.836909530733573776E-16, 0.000000000000000000 ) ) ;
#10813 = CARTESIAN_POINT ( 'NONE',  ( 12.72792205982779734, -12.72792206288791128, -22.63832499981969093 ) ) ;
#10814 = DIRECTION ( 'NONE',  ( -1.000000000000000000, -0.000000000000000000, -0.000000000000000000 ) ) ;
#10815 = ORIENTED_EDGE ( 'NONE', *, *, #410, .T. ) ;
#10816 = CARTESIAN_POINT ( 'NONE',  ( -10.00000000000000000, 0.000000000000000000, 0.000000000000000000 ) ) ;
#10817 = ORIENTED_EDGE ( 'NONE', *, *, #11547, .F. ) ;
#10818 = DIRECTION ( 'NONE',  ( 0.000000000000000000, 0.000000000000000000, -1.000000000000000000 ) ) ;
#10819 = CARTESIAN_POINT ( 'NONE',  ( 30.00000000000000000, -39.99999999999999289, -54.09999999999999432 ) ) ;
#10820 = ORIENTED_EDGE ( 'NONE', *, *, #962, .T. ) ;
#10821 = ORIENTED_EDGE ( 'NONE', *, *, #20770, .T. ) ;
#10822 = DIRECTION ( 'NONE',  ( -1.000000000000000000, 0.000000000000000000, 0.000000000000000000 ) ) ;
#10823 = FACE_OUTER_BOUND ( 'NONE', #5497, .T. ) ;
#10824 = DIRECTION ( 'NONE',  ( 0.000000000000000000, -0.000000000000000000, 1.000000000000000000 ) ) ;
#10825 = CARTESIAN_POINT ( 'NONE',  ( 9.474249098604504482, 6.330490856366291830, 17.91129649971319537 ) ) ;
#10826 = DIRECTION ( 'NONE',  ( 1.000000000000000000, 0.000000000000000000, 0.000000000000000000 ) ) ;
#10827 = CARTESIAN_POINT ( 'NONE',  ( 0.000000000000000000, 9.184850993605147944E-16, 7.500000000000000000 ) ) ;
#10828 = DIRECTION ( 'NONE',  ( 1.000000000000000000, 0.000000000000000000, 0.000000000000000000 ) ) ;
#10829 = AXIS2_PLACEMENT_3D ( 'NONE', #17771, #13308, #1860 ) ;
#10830 = ORIENTED_EDGE ( 'NONE', *, *, #9631, .F. ) ;
#10831 = CARTESIAN_POINT ( 'NONE',  ( 0.000000000000000000, 0.000000000000000000, -81.99999999999998579 ) ) ;
#10832 = VERTEX_POINT ( 'NONE', #11158 ) ;
#10833 = CARTESIAN_POINT ( 'NONE',  ( 15.25966316918061416, -10.19618095414378622, -5.987456249819688381 ) ) ;
#10834 = CARTESIAN_POINT ( 'NONE',  ( 21.45900938229203447, -1.326995226329893862, 84.99999999999998579 ) ) ;
#10835 = ORIENTED_EDGE ( 'NONE', *, *, #16284, .T. ) ;
#10836 = DIRECTION ( 'NONE',  ( 1.000000000000000000, 1.836909530733573776E-16, 0.000000000000000000 ) ) ;
#10837 = ORIENTED_EDGE ( 'NONE', *, *, #11038, .T. ) ;
#10838 = CARTESIAN_POINT ( 'NONE',  ( -5.303300859536632217, -5.303300858261584594, -5.516824999819692543 ) ) ;
#10839 = CARTESIAN_POINT ( 'NONE',  ( 7.500000000000002665, -9.015933403756338579E-10, -27.90119999981969556 ) ) ;
#10840 = LINE ( 'NONE', #6165, #905 ) ;
#10841 = ADVANCED_FACE ( 'NONE', ( #9052 ), #8984, .T. ) ;
#10842 = ORIENTED_EDGE ( 'NONE', *, *, #7290, .F. ) ;
#10843 = CARTESIAN_POINT ( 'NONE',  ( -9.850000000000012079, 0.000000000000000000, 46.00000000000000711 ) ) ;
#10844 = DIRECTION ( 'NONE',  ( 0.000000000000000000, 0.000000000000000000, 1.000000000000000000 ) ) ;
#10845 = CARTESIAN_POINT ( 'NONE',  ( -17.99999999999999645, 2.163826221265758470E-09, -21.00854999981969229 ) ) ;
#10846 = CARTESIAN_POINT ( 'NONE',  ( 0.000000000000000000, 0.000000000000000000, -5.294516984716111097 ) ) ;
#10847 = AXIS2_PLACEMENT_3D ( 'NONE', #14633, #6673, #5080 ) ;
#10848 = DIRECTION ( 'NONE',  ( 1.000000000000000000, 0.000000000000000000, 0.000000000000000000 ) ) ;
#10849 = VERTEX_POINT ( 'NONE', #5862 ) ;
#10850 = DIRECTION ( 'NONE',  ( -0.000000000000000000, -0.000000000000000000, 1.000000000000000000 ) ) ;
#10851 = CARTESIAN_POINT ( 'NONE',  ( 19.99999999999999645, 0.000000000000000000, 0.000000000000000000 ) ) ;
#10852 = CONICAL_SURFACE ( 'NONE', #4057, 2.055000000000000160, 0.7853981633974633780 ) ;
#10853 = ORIENTED_EDGE ( 'NONE', *, *, #1134, .T. ) ;
#10854 = CARTESIAN_POINT ( 'NONE',  ( -12.50000000000000533, 0.000000000000000000, 126.0000000000000000 ) ) ;
#10855 = CARTESIAN_POINT ( 'NONE',  ( -6.358192987158597376, 4.248408730893249441, -6.615206249819684636 ) ) ;
#10856 = ORIENTED_EDGE ( 'NONE', *, *, #11530, .T. ) ;
#10857 = CARTESIAN_POINT ( 'NONE',  ( -16.62983158437510056, 6.888301784570729502, -18.51488749981968951 ) ) ;
#10858 = DIRECTION ( 'NONE',  ( 0.000000000000000000, 0.000000000000000000, 1.000000000000000000 ) ) ;
#10859 = DIRECTION ( 'NONE',  ( 0.000000000000000000, 0.000000000000000000, -1.000000000000000000 ) ) ;
#10860 = VERTEX_POINT ( 'NONE', #1001 ) ;
#10861 = DIRECTION ( 'NONE',  ( -1.000000000000000000, 0.000000000000000000, 0.000000000000000000 ) ) ;
#10862 = ORIENTED_EDGE ( 'NONE', *, *, #16574, .T. ) ;
#10863 = FACE_OUTER_BOUND ( 'NONE', #5734, .T. ) ;
#10864 = EDGE_CURVE ( 'NONE', #17642, #6250, #9259, .T. ) ;
#10865 = AXIS2_PLACEMENT_3D ( 'NONE', #6612, #19556, #5032 ) ;
#10866 = ORIENTED_EDGE ( 'NONE', *, *, #653, .F. ) ;
#10867 = AXIS2_PLACEMENT_3D ( 'NONE', #4045, #13918, #10316 ) ;
#10868 = DIRECTION ( 'NONE',  ( 1.000000000000000000, 0.000000000000000000, 0.000000000000000000 ) ) ;
#10869 = EDGE_CURVE ( 'NONE', #714, #10217, #1217, .T. ) ;
#10870 = LINE ( 'NONE', #14267, #16024 ) ;
#10871 = CARTESIAN_POINT ( 'NONE',  ( -8.382925368423274293, 12.54593441764187745, 3.075448168841546703 ) ) ;
#10872 = ORIENTED_EDGE ( 'NONE', *, *, #17680, .F. ) ;
#10873 = DIRECTION ( 'NONE',  ( 0.000000000000000000, -7.039457583666960603E-15, 1.000000000000000000 ) ) ;
#10874 = ORIENTED_EDGE ( 'NONE', *, *, #16093, .T. ) ;
#10875 = CARTESIAN_POINT ( 'NONE',  ( 0.000000000000000000, -62.46228066917801414, 18.86519267363435048 ) ) ;
#10876 = VECTOR ( 'NONE', #1434, 1000.000000000000000 ) ;
#10877 = CARTESIAN_POINT ( 'NONE',  ( 12.72792206288790773, 12.72792205982779912, 10.80082500018031055 ) ) ;
#10878 = DIRECTION ( 'NONE',  ( -0.000000000000000000, -0.000000000000000000, 1.000000000000000000 ) ) ;
#10879 = CIRCLE ( 'NONE', #12225, 17.50000000000000355 ) ;
#10880 = DIRECTION ( 'NONE',  ( -1.000000000000000000, 0.000000000000000000, 0.000000000000000000 ) ) ;
#10881 = ORIENTED_EDGE ( 'NONE', *, *, #17373, .T. ) ;
#10882 = B_SPLINE_CURVE_WITH_KNOTS ( 'NONE', 3,
 ( #13198, #16268, #8512, #14686, #481, #10118 ),
 .UNSPECIFIED., .F., .F.,
 ( 4, 2, 4 ),
 ( 0.002336974151641604130, 0.003500975885716476211, 0.004664977619791348291 ),
 .UNSPECIFIED. ) ;
#10883 = CARTESIAN_POINT ( 'NONE',  ( -10.00000000000000000, 0.000000000000000000, 0.000000000000000000 ) ) ;
#10884 = CARTESIAN_POINT ( 'NONE',  ( 0.000000000000000000, 0.000000000000000000, -5.600000000000000533 ) ) ;
#10885 = VERTEX_POINT ( 'NONE', #6068 ) ;
#10886 = CARTESIAN_POINT ( 'NONE',  ( 21.29589421403332494, -8.772909163211549455, -84.50987075322080955 ) ) ;
#10887 = DIRECTION ( 'NONE',  ( -1.000000000000000000, -0.000000000000000000, 0.000000000000000000 ) ) ;
#10888 = CARTESIAN_POINT ( 'NONE',  ( 6.888301784570727726, 16.62983158437509701, -18.06323749981969584 ) ) ;
#10889 =( BOUNDED_CURVE ( )  B_SPLINE_CURVE ( 2, ( #17349, #9292, #7910, #14389, #15753, #14181, #20831, #12897, #6315, #11297, #2714, #1141, #16375, #11713, #1668, #3438, #9804 ),
 .UNSPECIFIED., .F., .F. ) 
 B_SPLINE_CURVE_WITH_KNOTS ( ( 3, 2, 2, 2, 2, 2, 2, 2, 3 ),
 ( 0.9000000000038511638, 0.9125000000033697267, 0.9250000000028884006, 0.9375000000024069635, 0.9500000000019255264, 0.9625000000014442003, 0.9750000000009627632, 0.9875000000004814371, 1.000000000000000000 ),
 .UNSPECIFIED. ) 
 CURVE ( )  GEOMETRIC_REPRESENTATION_ITEM ( )  RATIONAL_B_SPLINE_CURVE ( ( 0.9999999999940800688, 0.9807852804091503618, 1.000000000000000000, 0.9807852804032304306, 1.000000000000000000, 0.9807852804032304306, 1.000000000000000000, 0.9807852804032304306, 1.000000000000000000, 0.9807852804032304306, 1.000000000000000000, 0.9807852804032304306, 1.000000000000000000, 0.9807852804032304306, 1.000000000000000000, 0.9807852804032304306, 1.000000000000000000 ) ) 
 REPRESENTATION_ITEM ( '' )  );
#10890 = ORIENTED_EDGE ( 'NONE', *, *, #1838, .F. ) ;
#10891 = CARTESIAN_POINT ( 'NONE',  ( 19.99999999999999645, 60.40676135667438729, 23.56039007469059143 ) ) ;
#10892 = EDGE_CURVE ( 'NONE', #510, #9981, #12316, .T. ) ;
#10893 = DIRECTION ( 'NONE',  ( 1.000000000000000000, -0.000000000000000000, -0.000000000000000000 ) ) ;
#10894 = EDGE_CURVE ( 'NONE', #4551, #20902, #19806, .T. ) ;
#10895 = DIRECTION ( 'NONE',  ( -1.000000000000000000, 0.000000000000000000, 0.000000000000000000 ) ) ;
#10896 = CARTESIAN_POINT ( 'NONE',  ( 19.99999999999999645, -31.98952867950364265, 56.39803944231574206 ) ) ;
#10897 = CIRCLE ( 'NONE', #6142, 2.649999999999999467 ) ;
#10898 = CARTESIAN_POINT ( 'NONE',  ( 0.000000000000000000, 0.000000000000000000, -212.0000000000000284 ) ) ;
#10899 = CARTESIAN_POINT ( 'NONE',  ( -12.72792205982780089, 12.72792206288791128, 10.34917500018030978 ) ) ;
#10900 = CARTESIAN_POINT ( 'NONE',  ( 2.870125741905214412, -6.929096494179682431, -10.44411249981968481 ) ) ;
#10901 = EDGE_CURVE ( 'NONE', #14245, #10263, #1559, .T. ) ;
#10902 = ORIENTED_EDGE ( 'NONE', *, *, #19809, .T. ) ;
#10903 = DIRECTION ( 'NONE',  ( 0.000000000000000000, 0.000000000000000000, 1.000000000000000000 ) ) ;
#10904 = CARTESIAN_POINT ( 'NONE',  ( -13.67243654778935102, -5.663308646854334327, 14.24564558151907789 ) ) ;
#10905 = AXIS2_PLACEMENT_3D ( 'NONE', #16524, #16037, #13459 ) ;
#10906 = VERTEX_POINT ( 'NONE', #12642 ) ;
#10907 = DIRECTION ( 'NONE',  ( 0.000000000000000000, 0.000000000000000000, 1.000000000000000000 ) ) ;
#10908 = CARTESIAN_POINT ( 'NONE',  ( 16.62983158437509346, -6.888301784570739272, -23.22738749981969164 ) ) ;
#10909 = CARTESIAN_POINT ( 'NONE',  ( 30.00000000000000000, -105.0000000000000000, 72.35596062816881613 ) ) ;
#10910 = CIRCLE ( 'NONE', #4119, 65.24900000006526568 ) ;
#10911 = ORIENTED_EDGE ( 'NONE', *, *, #668, .T. ) ;
#10912 = EDGE_CURVE ( 'NONE', #19648, #17002, #9687, .T. ) ;
#10913 = DIRECTION ( 'NONE',  ( -1.000000000000000000, -0.000000000000000000, 0.000000000000000000 ) ) ;
#10914 = ORIENTED_EDGE ( 'NONE', *, *, #3080, .T. ) ;
#10915 = CARTESIAN_POINT ( 'NONE',  ( 37.45104809098000942, -20.09218443038071200, -76.71572404264729528 ) ) ;
#10916 = DIRECTION ( 'NONE',  ( 0.000000000000000000, 0.000000000000000000, 1.000000000000000000 ) ) ;
#10917 = ORIENTED_EDGE ( 'NONE', *, *, #2765, .T. ) ;
#10918 = ORIENTED_EDGE ( 'NONE', *, *, #19061, .T. ) ;
#10919 = CARTESIAN_POINT ( 'NONE',  ( 34.73553668442697528, -117.9508568039212832, -77.26256316625480736 ) ) ;
#10920 = EDGE_CURVE ( 'NONE', #12091, #8697, #18897, .T. ) ;
#10921 = EDGE_CURVE ( 'NONE', #14352, #1061, #15700, .T. ) ;
#10922 = DIRECTION ( 'NONE',  ( 0.000000000000000000, 0.9422609221188213979, -0.3348796121709836093 ) ) ;
#10923 = CIRCLE ( 'NONE', #13631, 2.649999999999999467 ) ;
#10924 = AXIS2_PLACEMENT_3D ( 'NONE', #16799, #688, #10445 ) ;
#10925 = EDGE_CURVE ( 'NONE', #15704, #15337, #17131, .T. ) ;
#10926 = AXIS2_PLACEMENT_3D ( 'NONE', #2716, #17351, #20416 ) ;
#10927 = AXIS2_PLACEMENT_3D ( 'NONE', #16694, #8635, #11921 ) ;
#10928 = CARTESIAN_POINT ( 'NONE',  ( 7.499999999820660790, -1.491842756249031954, -27.60666874981969343 ) ) ;
#10929 = CYLINDRICAL_SURFACE ( 'NONE', #18679, 27.60000000002760245 ) ;
#10930 = AXIS2_PLACEMENT_3D ( 'NONE', #13098, #1666, #6410 ) ;
#10931 = CARTESIAN_POINT ( 'NONE',  ( 0.000000000000000000, 0.000000000000000000, -5.600000000000000533 ) ) ;
#10932 = DIRECTION ( 'NONE',  ( 1.000000000000000000, 0.000000000000000000, 0.000000000000000000 ) ) ;
#10933 = ORIENTED_EDGE ( 'NONE', *, *, #20220, .F. ) ;
#10934 = CARTESIAN_POINT ( 'NONE',  ( 30.00000000000000000, -85.00000000000000000, -1.040949779275250179E-14 ) ) ;
#10935 = VERTEX_POINT ( 'NONE', #20670 ) ;
#10936 = CARTESIAN_POINT ( 'NONE',  ( 15.25966316918061416, -10.19618095414378622, -15.41245624981968732 ) ) ;
#10937 = CARTESIAN_POINT ( 'NONE',  ( 15.37884418493264782, -15.02891098528242431, 73.77646566961476537 ) ) ;
#10938 = CIRCLE ( 'NONE', #454, 27.60000000002759890 ) ;
#10939 = ORIENTED_EDGE ( 'NONE', *, *, #799, .T. ) ;
#10940 = EDGE_CURVE ( 'NONE', #8249, #7867, #20254, .T. ) ;
#10941 = DIRECTION ( 'NONE',  ( 1.000000000000000000, 0.000000000000000000, 0.000000000000000000 ) ) ;
#10942 = VERTEX_POINT ( 'NONE', #4142 ) ;
#10943 = FACE_BOUND ( 'NONE', #18792, .T. ) ;
#10944 = CARTESIAN_POINT ( 'NONE',  ( 0.000000000000000000, 0.000000000000000000, 0.000000000000000000 ) ) ;
#10945 = CARTESIAN_POINT ( 'NONE',  ( 19.99999999999999645, 70.29359119158485214, 15.58239511117312226 ) ) ;
#10946 = VERTEX_POINT ( 'NONE', #6053 ) ;
#10947 = CARTESIAN_POINT ( 'NONE',  ( -44.00000000000000000, -85.00000000000000000, 11.49999999999998579 ) ) ;
#10948 = AXIS2_PLACEMENT_3D ( 'NONE', #18881, #4352, #4561 ) ;
#10949 = CARTESIAN_POINT ( 'NONE',  ( 19.99999999999999645, 31.17893654894306721, -57.31758819669140337 ) ) ;
#10950 = LINE ( 'NONE', #1325, #12023 ) ;
#10951 = LINE ( 'NONE', #18913, #8594 ) ;
#10952 = CIRCLE ( 'NONE', #2495, 80.00000000000000000 ) ;
#10953 = DIRECTION ( 'NONE',  ( 1.000000000000000000, 0.000000000000000000, 0.000000000000000000 ) ) ;
#10954 = AXIS2_PLACEMENT_3D ( 'NONE', #1220, #15832, #7669 ) ;
#10956 = EDGE_LOOP ( 'NONE', ( #10151, #16459, #11459, #9897 ) ) ;
#10955 = CIRCLE ( 'NONE', #16043, 72.00000000007199219 ) ;
#10957 = CARTESIAN_POINT ( 'NONE',  ( 0.000000000000000000, -36.54710069451017063, -54.05313526368150434 ) ) ;
#10958 = EDGE_CURVE ( 'NONE', #14005, #1037, #6956, .T. ) ;
#10959 = DIRECTION ( 'NONE',  ( 0.000000000000000000, 0.000000000000000000, 1.000000000000000000 ) ) ;
#10960 = ORIENTED_EDGE ( 'NONE', *, *, #1629, .T. ) ;
#10961 = DIRECTION ( 'NONE',  ( 0.000000000000000000, 0.000000000000000000, 1.000000000000000000 ) ) ;
#10962 = CARTESIAN_POINT ( 'NONE',  ( 0.000000000000000000, 0.000000000000000000, 0.000000000000000000 ) ) ;
#10963 = ORIENTED_EDGE ( 'NONE', *, *, #19234, .T. ) ;
#10964 = CARTESIAN_POINT ( 'NONE',  ( -12.72792205982779912, 12.72792206288790950, -8.500824999819686312 ) ) ;
#10965 = DIRECTION ( 'NONE',  ( 0.000000000000000000, 0.000000000000000000, 1.000000000000000000 ) ) ;
#10966 = CARTESIAN_POINT ( 'NONE',  ( 1.084202172485504434E-14, 4.618802153517020059, -0.3572655899081733644 ) ) ;
#10967 = AXIS2_PLACEMENT_3D ( 'NONE', #16656, #8603, #13492 ) ;
#10968 = ORIENTED_EDGE ( 'NONE', *, *, #13888, .T. ) ;
#10969 = VECTOR ( 'NONE', #12915, 1000.000000000000000 ) ;
#10970 = DIRECTION ( 'NONE',  ( 1.000000000000000000, 0.000000000000000000, 0.000000000000000000 ) ) ;
#10971 = ORIENTED_EDGE ( 'NONE', *, *, #1806, .F. ) ;
#10972 = PLANE ( 'NONE',  #18329 ) ;
#10973 = AXIS2_PLACEMENT_3D ( 'NONE', #12101, #449, #11781 ) ;
#10974 = LINE ( 'NONE', #17016, #3316 ) ;
#10975 = DIRECTION ( 'NONE',  ( 0.000000000000000000, 0.000000000000000000, -1.000000000000000000 ) ) ;
#10976 = CONTEXT_DEPENDENT_SHAPE_REPRESENTATION ( #478, #5423 ) ;
#10977 = CIRCLE ( 'NONE', #11651, 39.99999999999999289 ) ;
#10978 = CARTESIAN_POINT ( 'NONE',  ( 1.779017513685136568E-09, 14.79893867758297610, -5.465958081158456494 ) ) ;
#10979 = ORIENTED_EDGE ( 'NONE', *, *, #12855, .T. ) ;
#10980 = CARTESIAN_POINT ( 'NONE',  ( -7.500000000000004441, -1.491842754878798916, -14.05823124991221285 ) ) ;
#10981 = EDGE_CURVE ( 'NONE', #4783, #13795, #3900, .T. ) ;
#10982 = LINE ( 'NONE', #15860, #17061 ) ;
#10983 = VERTEX_POINT ( 'NONE', #17297 ) ;
#10984 = CARTESIAN_POINT ( 'NONE',  ( 20.20955665649389843, -7.405347705393168667, 85.81428755717244883 ) ) ;
#10985 = CARTESIAN_POINT ( 'NONE',  ( -6.888301784570736608, -16.62983158437509346, 5.499262500180311264 ) ) ;
#10986 = CARTESIAN_POINT ( 'NONE',  ( -2.870125741905210415, 6.929096494179677990, -21.42151249981969130 ) ) ;
#10987 = CYLINDRICAL_SURFACE ( 'NONE', #13077, 4.250000000000000000 ) ;
#10988 = ORIENTED_EDGE ( 'NONE', *, *, #20220, .T. ) ;
#10989 = LINE ( 'NONE', #18947, #17517 ) ;
#10990 = DIRECTION ( 'NONE',  ( 1.000000000000000000, 0.000000000000000000, 0.000000000000000000 ) ) ;
#10991 = ORIENTED_EDGE ( 'NONE', *, *, #12420, .F. ) ;
#10992 = CARTESIAN_POINT ( 'NONE',  ( -21.27651084028035910, -8.819135707481013497, -84.46788585316646447 ) ) ;
#10993 = CARTESIAN_POINT ( 'NONE',  ( -6.929096494179678878, -2.870125741905209971, 4.497237500180307990 ) ) ;
#10994 = CARTESIAN_POINT ( 'NONE',  ( -16.62983158603121936, -6.888301780572499311, -21.59761249981969300 ) ) ;
#10995 = VERTEX_POINT ( 'NONE', #7855 ) ;
#10996 = CARTESIAN_POINT ( 'NONE',  ( -2.870125743571144028, -6.929096493489630859, -9.265987499819688722 ) ) ;
#10997 = COLOUR_RGB ( '', 0.72549020, 0.75294118, 0.79215686) ;
#10998 = CARTESIAN_POINT ( 'NONE',  ( 19.99999999999999645, 0.000000000000000000, 0.000000000000000000 ) ) ;
#10999 = FACE_OUTER_BOUND ( 'NONE', #13050, .T. ) ;
#11000 = DIRECTION ( 'NONE',  ( 1.000000000000000000, 0.000000000000000000, 0.000000000000000000 ) ) ;
#11001 = DIRECTION ( 'NONE',  ( -1.224646799147353207E-16, 0.000000000000000000, -1.000000000000000000 ) ) ;
#11002 = CARTESIAN_POINT ( 'NONE',  ( -16.62983158603122646, -6.888301780572501976, 8.581987500180309425 ) ) ;
#11003 = CARTESIAN_POINT ( 'NONE',  ( -7.500000000179346316, -1.491842754445844355, -17.21833124981968766 ) ) ;
#11004 = VERTEX_POINT ( 'NONE', #11037 ) ;
#11005 = ORIENTED_EDGE ( 'NONE', *, *, #17189, .T. ) ;
#11006 = CARTESIAN_POINT ( 'NONE',  ( -4.000000000000000000, 2.309401076758496263, -5.599999999999999645 ) ) ;
#11007 = CARTESIAN_POINT ( 'NONE',  ( -12.54593441562640166, 8.382925371439625906, 15.71830183151907612 ) ) ;
#11008 = DIRECTION ( 'NONE',  ( -1.000000000000000000, 0.000000000000000000, 0.000000000000000000 ) ) ;
#11009 = EDGE_CURVE ( 'NONE', #8953, #8874, #17410, .T. ) ;
#11010 = AXIS2_PLACEMENT_3D ( 'NONE', #12442, #20687, #14355 ) ;
#11011 = VERTEX_POINT ( 'NONE', #2988 ) ;
#11012 = PLANE ( 'NONE',  #6184 ) ;
#11013 = EDGE_CURVE ( 'NONE', #13722, #18976, #190, .T. ) ;
#11014 = CARTESIAN_POINT ( 'NONE',  ( -18.00000000043041126, -3.580422610670022543, -19.39848124981969235 ) ) ;
#11015 = CARTESIAN_POINT ( 'NONE',  ( 19.99999999999999645, -59.36728637278046250, 40.73727173906767973 ) ) ;
#11016 = SHAPE_REPRESENTATION ( 'socket head cap screw_iso_ISO 4762 M5 x 12 - 12N', ( #12461 ), #19129 ) ;
#11017 = EDGE_LOOP ( 'NONE', ( #12400, #17577, #12163, #12667 ) ) ;
#11018 = LINE ( 'NONE', #1499, #17347 ) ;
#11019 = ORIENTED_EDGE ( 'NONE', *, *, #5565, .T. ) ;
#11020 = CARTESIAN_POINT ( 'NONE',  ( 30.89068055997971385, -39.25147108719813360, -71.46578918091849175 ) ) ;
#11021 = LINE ( 'NONE', #10819, #19730 ) ;
#11022 = ORIENTED_EDGE ( 'NONE', *, *, #19178, .T. ) ;
#11023 = EDGE_CURVE ( 'NONE', #19012, #10641, #9448, .T. ) ;
#11024 = ORIENTED_EDGE ( 'NONE', *, *, #5354, .F. ) ;
#11025 = CARTESIAN_POINT ( 'NONE',  ( 19.99999999999999645, -31.17893654894190902, -57.31758819669202865 ) ) ;
#11026 = AXIS2_PLACEMENT_3D ( 'NONE', #1769, #11313, #9917 ) ;
#11027 = B_SPLINE_CURVE_WITH_KNOTS ( 'NONE', 3,
 ( #916, #12566, #12363, #13844, #9284, #12469, #4303, #10775, #15633, #7584, #20512, #15745, #1242, #14172, #1659, #1554, #8306, #6503, #4923, #9795 ),
 .UNSPECIFIED., .F., .F.,
 ( 4, 2, 2, 2, 2, 2, 2, 2, 2, 4 ),
 ( 0.000000000000000000, 0.005578321817708520487, 0.006972902272135647790, 0.008367482726562769021, 0.01115664363541698026, 0.01255122408984410062, 0.01394580454427121752, 0.01673496545312545478, 0.01952412636197969203, 0.02231328727083392929 ),
 .UNSPECIFIED. ) ;
#11028 =( NAMED_UNIT ( * ) SI_UNIT ( $, .STERADIAN. ) SOLID_ANGLE_UNIT ( ) );
#11029 = PLANE ( 'NONE',  #15004 ) ;
#11030 = AXIS2_PLACEMENT_3D ( 'NONE', #19202, #6461, #1516 ) ;
#11031 = CARTESIAN_POINT ( 'NONE',  ( 0.000000000000000000, -63.85430960833482317, -11.25592921604904539 ) ) ;
#11032 = CARTESIAN_POINT ( 'NONE',  ( 10.32494394706616347, -4.276731815070950127, -11.19332774935257468 ) ) ;
#11033 = EDGE_CURVE ( 'NONE', #4233, #15895, #17086, .T. ) ;
#11034 = CARTESIAN_POINT ( 'NONE',  ( -6.929096493489625530, 2.870125743571138255, -22.59963749981969272 ) ) ;
#11035 = CARTESIAN_POINT ( 'NONE',  ( 6.249999999999902300, -10.82531754730554496, 43.00000000000000000 ) ) ;
#11036 = CYLINDRICAL_SURFACE ( 'NONE', #15444, 27.60000000002759890 ) ;
#11037 = CARTESIAN_POINT ( 'NONE',  ( 52.50000000000000000, -130.0000000000000000, 5.000000000000000000 ) ) ;
#11038 = EDGE_CURVE ( 'NONE', #13702, #2306, #17821, .T. ) ;
#11039 = AXIS2_PLACEMENT_3D ( 'NONE', #2735, #12713, #4744 ) ;
#11040 = ORIENTED_EDGE ( 'NONE', *, *, #14301, .T. ) ;
#11041 = FACE_OUTER_BOUND ( 'NONE', #689, .T. ) ;
#11042 = VECTOR ( 'NONE', #17844, 1000.000000000000000 ) ;
#11043 = EDGE_CURVE ( 'NONE', #2557, #2098, #12424, .T. ) ;
#11044 = ORIENTED_EDGE ( 'NONE', *, *, #16591, .T. ) ;
#11045 = CARTESIAN_POINT ( 'NONE',  ( 17.99999999956958163, -3.580422614997676334, -16.00151874981968803 ) ) ;
#11046 = CARTESIAN_POINT ( 'NONE',  ( 50.00000000000000000, -42.57363661491096707, -121.3828884801879155 ) ) ;
#11047 = ORIENTED_EDGE ( 'NONE', *, *, #399, .T. ) ;
#11048 = DIRECTION ( 'NONE',  ( -1.000000000000000000, -0.000000000000000000, -0.000000000000000000 ) ) ;
#11049 = CIRCLE ( 'NONE', #19497, 72.00000000007199219 ) ;
#11050 = ORIENTED_EDGE ( 'NONE', *, *, #2855, .F. ) ;
#11051 = AXIS2_PLACEMENT_3D ( 'NONE', #13361, #10278, #10073 ) ;
#11052 = CARTESIAN_POINT ( 'NONE',  ( -25.00000000000000000, -30.00000000000000711, 50.99019513592783426 ) ) ;
#11053 = DIRECTION ( 'NONE',  ( 0.000000000000000000, -1.000000000000000000, -0.000000000000000000 ) ) ;
#11054 = CARTESIAN_POINT ( 'NONE',  ( 1.491842756249029289, 7.499999999820664343, -1.687918749819692588 ) ) ;
#11055 = ADVANCED_FACE ( 'NONE', ( #18785 ), #4254, .T. ) ;
#11056 = VERTEX_POINT ( 'NONE', #9133 ) ;
#11057 = DIRECTION ( 'NONE',  ( 0.000000000000000000, 0.9422609221188191775, 0.3348796121709899376 ) ) ;
#11058 = AXIS2_PLACEMENT_3D ( 'NONE', #6380, #19116, #4694 ) ;
#11059 = CARTESIAN_POINT ( 'NONE',  ( 52.50000000000000000, -120.0000000000000142, 5.000000000000000000 ) ) ;
#11060 = CARTESIAN_POINT ( 'NONE',  ( 6.250000000000054179, 10.82531754730546147, -43.00000000000000000 ) ) ;
#11061 = VECTOR ( 'NONE', #16988, 1000.000000000000000 ) ;
#11062 = CIRCLE ( 'NONE', #4626, 23.00000000000000000 ) ;
#11063 = CARTESIAN_POINT ( 'NONE',  ( 6.929096493489625530, -2.870125743571142252, 10.38786250018030799 ) ) ;
#11064 = EDGE_CURVE ( 'NONE', #8436, #3519, #2238, .T. ) ;
#11065 = ORIENTED_EDGE ( 'NONE', *, *, #17288, .F. ) ;
#11066 = ADVANCED_FACE ( 'NONE', ( #8266 ), #9852, .T. ) ;
#11067 = AXIS2_PLACEMENT_3D ( 'NONE', #11581, #11384, #16557 ) ;
#11068 = CIRCLE ( 'NONE', #7672, 72.00000000007199219 ) ;
#11069 = EDGE_CURVE ( 'NONE', #1553, #15627, #9335, .T. ) ;
#11070 = CARTESIAN_POINT ( 'NONE',  ( 19.99999999999999645, 36.54710069451054011, 54.05313526368126276 ) ) ;
#11071 = CARTESIAN_POINT ( 'NONE',  ( -6.929096494179684207, -2.870125741905212635, 1.337137500180316074 ) ) ;
#11072 = ORIENTED_EDGE ( 'NONE', *, *, #19926, .T. ) ;
#11073 = DIRECTION ( 'NONE',  ( -1.000000000000000000, -0.000000000000000000, -0.000000000000000000 ) ) ;
#11074 = DIRECTION ( 'NONE',  ( 0.000000000000000000, 0.000000000000000000, -1.000000000000000000 ) ) ;
#11075 = ORIENTED_EDGE ( 'NONE', *, *, #2147, .F. ) ;
#11076 = CARTESIAN_POINT ( 'NONE',  ( -16.62983158437510056, 6.888301784570729502, -9.089887499819687022 ) ) ;
#11077 = ADVANCED_FACE ( 'NONE', ( #3083 ), #7967, .T. ) ;
#11078 = VECTOR ( 'NONE', #972, 1000.000000000000000 ) ;
#11079 = DIRECTION ( 'NONE',  ( -1.000000000000000000, -0.000000000000000000, -0.000000000000000000 ) ) ;
#11080 = CARTESIAN_POINT ( 'NONE',  ( 19.99999999999999645, 0.000000000000000000, 0.000000000000000000 ) ) ;
#11081 = ORIENTED_EDGE ( 'NONE', *, *, #5311, .T. ) ;
#11082 = DIRECTION ( 'NONE',  ( 1.000000000000000000, 1.836909530733573776E-16, 0.000000000000000000 ) ) ;
#11083 = EDGE_LOOP ( 'NONE', ( #19083, #10610, #12108, #6271 ) ) ;
#11084 = DIRECTION ( 'NONE',  ( -0.000000000000000000, -1.000000000000000000, -0.000000000000000000 ) ) ;
#11085 = AXIS2_PLACEMENT_3D ( 'NONE', #12385, #7722, #15549 ) ;
#11086 = ORIENTED_EDGE ( 'NONE', *, *, #9023, .F. ) ;
#11087 = AXIS2_PLACEMENT_3D ( 'NONE', #13009, #9914, #1673 ) ;
#11088 = AXIS2_PLACEMENT_3D ( 'NONE', #4774, #12947, #9851 ) ;
#11089 = DIRECTION ( 'NONE',  ( 1.000000000000000000, -0.000000000000000000, -0.000000000000000000 ) ) ;
#11090 = CYLINDRICAL_SURFACE ( 'NONE', #9593, 27.60000000002760245 ) ;
#11091 = CARTESIAN_POINT ( 'NONE',  ( -11.17563879704982988, 2.222972771497744748, 21.49964100064742922 ) ) ;
#11092 = ORIENTED_EDGE ( 'NONE', *, *, #11279, .F. ) ;
#11093 = CARTESIAN_POINT ( 'NONE',  ( 6.929096493489625530, -2.870125743571142252, -17.88713749981969414 ) ) ;
#11094 = AXIS2_PLACEMENT_3D ( 'NONE', #17871, #11089, #7896 ) ;
#11095 = CARTESIAN_POINT ( 'NONE',  ( 8.900000000000041211, 10.82531754730546147, 126.0000000000000000 ) ) ;
#11096 = ORIENTED_EDGE ( 'NONE', *, *, #6726, .T. ) ;
#11097 = DIRECTION ( 'NONE',  ( -1.000000000000000000, 0.000000000000000000, -0.000000000000000000 ) ) ;
#11098 = AXIS2_PLACEMENT_3D ( 'NONE', #8134, #7824, #20549 ) ;
#11099 = LINE ( 'NONE', #19152, #16614 ) ;
#11100 = CARTESIAN_POINT ( 'NONE',  ( 0.000000000000000000, -49.77519642624037743, 42.18840861821767874 ) ) ;
#11101 = ORIENTED_EDGE ( 'NONE', *, *, #2050, .F. ) ;
#11102 = LINE ( 'NONE', #8024, #12793 ) ;
#11103 = DIRECTION ( 'NONE',  ( 0.000000000000000000, 0.000000000000000000, 1.000000000000000000 ) ) ;
#11104 = ORIENTED_EDGE ( 'NONE', *, *, #13351, .T. ) ;
#11105 = DIRECTION ( 'NONE',  ( 1.000000000000000000, 1.836909530733573776E-16, 0.000000000000000000 ) ) ;
#11106 = EDGE_CURVE ( 'NONE', #12251, #273, #3569, .T. ) ;
#11107 = CARTESIAN_POINT ( 'NONE',  ( 1.084202172485504434E-14, 4.618802153517020059, -5.242734410091827613 ) ) ;
#11108 = LINE ( 'NONE', #14703, #11620 ) ;
#11109 = ADVANCED_FACE ( 'NONE', ( #1813 ), #14336, .T. ) ;
#11110 = AXIS2_PLACEMENT_3D ( 'NONE', #18911, #5746, #19006 ) ;
#11111 = ORIENTED_EDGE ( 'NONE', *, *, #14047, .F. ) ;
#11112 = CARTESIAN_POINT ( 'NONE',  ( 6.679999999999998828, 7.059243326609123303E-15, 0.000000000000000000 ) ) ;
#11113 = DIRECTION ( 'NONE',  ( 0.000000000000000000, -0.9976687691905385957, -0.06824241336468162000 ) ) ;
#11114 = DIRECTION ( 'NONE',  ( 0.000000000000000000, 0.000000000000000000, 1.000000000000000000 ) ) ;
#11115 = CARTESIAN_POINT ( 'NONE',  ( 10.19618095047498052, -15.25966317163203456, -12.91879374981968986 ) ) ;
#11116 = CARTESIAN_POINT ( 'NONE',  ( -5.303300858261589035, 5.303300859536635770, -15.74567499981968588 ) ) ;
#11117 = ORIENTED_EDGE ( 'NONE', *, *, #13247, .F. ) ;
#11118 = LINE ( 'NONE', #16199, #14148 ) ;
#11119 = CARTESIAN_POINT ( 'NONE',  ( -8.382925368423267187, 12.54593441764186856, 16.30736433151907860 ) ) ;
#11120 = DIRECTION ( 'NONE',  ( 0.000000000000000000, 0.000000000000000000, 1.000000000000000000 ) ) ;
#11121 = ORIENTED_EDGE ( 'NONE', *, *, #2175, .T. ) ;
#11122 = DIRECTION ( 'NONE',  ( 1.000000000000000000, -0.000000000000000000, -0.000000000000000000 ) ) ;
#11123 = CARTESIAN_POINT ( 'NONE',  ( -3.580422610670018546, 18.00000000043041126, -17.04223124981968951 ) ) ;
#11124 = CARTESIAN_POINT ( 'NONE',  ( 19.99999999999999645, 0.000000000000000000, 0.000000000000000000 ) ) ;
#11125 = ORIENTED_EDGE ( 'NONE', *, *, #17128, .F. ) ;
#11126 = CARTESIAN_POINT ( 'NONE',  ( 6.232799999999998342, 10.79377999999999993, 0.000000000000000000 ) ) ;
#11127 = ORIENTED_EDGE ( 'NONE', *, *, #7546, .F. ) ;
#11128 = CARTESIAN_POINT ( 'NONE',  ( 31.38212025810754824, -36.77472472338947540, -71.71337048941178693 ) ) ;
#11129 = DIRECTION ( 'NONE',  ( -1.000000000000000000, 0.000000000000000000, -0.000000000000000000 ) ) ;
#11130 = EDGE_CURVE ( 'NONE', #3436, #8121, #11545, .T. ) ;
#11131 = ORIENTED_EDGE ( 'NONE', *, *, #504, .T. ) ;
#11132 = ORIENTED_EDGE ( 'NONE', *, *, #5387, .T. ) ;
#11133 = LINE ( 'NONE', #3072, #14122 ) ;
#11135 = EDGE_CURVE ( 'NONE', #764, #8758, #20783, .T. ) ;
#11134 = DIRECTION ( 'NONE',  ( -1.000000000000000000, 0.000000000000000000, -0.000000000000000000 ) ) ;
#11136 = EDGE_CURVE ( 'NONE', #3825, #15895, #7296, .T. ) ;
#11137 = DIRECTION ( 'NONE',  ( 0.000000000000000000, 0.000000000000000000, 1.000000000000000000 ) ) ;
#11138 = CARTESIAN_POINT ( 'NONE',  ( -7.902369976724401113, 7.902369978624329327, -5.891765249352570954 ) ) ;
#11139 = CARTESIAN_POINT ( 'NONE',  ( -10.32494394706615815, 4.276731815070940357, 14.67145274971319857 ) ) ;
#11140 = CARTESIAN_POINT ( 'NONE',  ( -44.00000000000000000, -85.00000000000000000, -1.040949779275250179E-14 ) ) ;
#11141 = CARTESIAN_POINT ( 'NONE',  ( 19.99999999999999645, 18.50424539729942808, -69.58155576219097327 ) ) ;
#11142 = CARTESIAN_POINT ( 'NONE',  ( -62.49999999999999289, -30.00000000000000000, 0.000000000000000000 ) ) ;
#11143 = EDGE_CURVE ( 'NONE', #2306, #13702, #16439, .T. ) ;
#11144 = VERTEX_POINT ( 'NONE', #1910 ) ;
#11145 = DIRECTION ( 'NONE',  ( 0.000000000000000000, 0.000000000000000000, -1.000000000000000000 ) ) ;
#11146 = ORIENTED_EDGE ( 'NONE', *, *, #9984, .F. ) ;
#11147 = CARTESIAN_POINT ( 'NONE',  ( -18.00000000000000000, 2.163826221265758884E-09, -21.00854999981968874 ) ) ;
#11148 = DIRECTION ( 'NONE',  ( 1.000000000000000000, 0.000000000000000000, 0.000000000000000000 ) ) ;
#11149 = ORIENTED_EDGE ( 'NONE', *, *, #2866, .T. ) ;
#11150 = CARTESIAN_POINT ( 'NONE',  ( -8.500000000000000000, 0.000000000000000000, -81.99999999999998579 ) ) ;
#11151 = ORIENTED_EDGE ( 'NONE', *, *, #20367, .T. ) ;
#11152 = LINE ( 'NONE', #9251, #694 ) ;
#11153 = FACE_OUTER_BOUND ( 'NONE', #14960, .T. ) ;
#11154 = CARTESIAN_POINT ( 'NONE',  ( 30.00000000000000000, -85.00000000000000000, -1.040949779275250179E-14 ) ) ;
#11155 = APPLICATION_CONTEXT ( 'automotive_design' ) ;
#11156 = ORIENTED_EDGE ( 'NONE', *, *, #16824, .T. ) ;
#11157 = CYLINDRICAL_SURFACE ( 'NONE', #2232, 65.24900000006525147 ) ;
#11158 = CARTESIAN_POINT ( 'NONE',  ( 25.00000000000000711, -29.99999999999999645, -45.00000000000000000 ) ) ;
#11159 = DIRECTION ( 'NONE',  ( 0.000000000000000000, 0.000000000000000000, -1.000000000000000000 ) ) ;
#11160 = EDGE_CURVE ( 'NONE', #20507, #10032, #20151, .T. ) ;
#11161 = ADVANCED_FACE ( 'NONE', ( #14634 ), #11458, .T. ) ;
#11162 = DIRECTION ( 'NONE',  ( -1.000000000000000000, 0.000000000000000000, 0.000000000000000000 ) ) ;
#11163 = VERTEX_POINT ( 'NONE', #17612 ) ;
#11164 = CARTESIAN_POINT ( 'NONE',  ( -9.850000000000006750, 0.000000000000000000, 43.00000000000000000 ) ) ;
#11165 = EDGE_CURVE ( 'NONE', #14747, #14238, #3387, .T. ) ;
#11166 = CARTESIAN_POINT ( 'NONE',  ( 4.248408729364579806, -6.358192988180021210, -1.313643749819685347 ) ) ;
#11167 = ORIENTED_EDGE ( 'NONE', *, *, #2496, .T. ) ;
#11168 = EDGE_CURVE ( 'NONE', #10860, #13107, #216, .T. ) ;
#11169 = LINE ( 'NONE', #1118, #15696 ) ;
#11170 = DIRECTION ( 'NONE',  ( -1.000000000000000000, 0.000000000000000000, 0.000000000000000000 ) ) ;
#11171 = ORIENTED_EDGE ( 'NONE', *, *, #11136, .F. ) ;
#11172 = CARTESIAN_POINT ( 'NONE',  ( 17.99999999956958163, -3.580422614997676334, -23.52191874981969022 ) ) ;
#11173 = DIRECTION ( 'NONE',  ( -1.000000000000000000, -0.000000000000000000, 0.000000000000000000 ) ) ;
#11174 = DIRECTION ( 'NONE',  ( -1.000000000000000000, 0.000000000000000000, 0.000000000000000000 ) ) ;
#11175 = ORIENTED_EDGE ( 'NONE', *, *, #18305, .F. ) ;
#11176 = DIRECTION ( 'NONE',  ( -0.000000000000000000, -0.000000000000000000, 1.000000000000000000 ) ) ;
#11177 = ORIENTED_EDGE ( 'NONE', *, *, #7290, .T. ) ;
#11178 = LINE ( 'NONE', #15943, #13271 ) ;
#11179 = EDGE_CURVE ( 'NONE', #540, #7659, #3250, .T. ) ;
#11180 = ORIENTED_EDGE ( 'NONE', *, *, #15687, .F. ) ;
#11181 = ADVANCED_FACE ( 'NONE', ( #16018 ), #13155, .F. ) ;
#11182 = CYLINDRICAL_SURFACE ( 'NONE', #13802, 72.00000000007199219 ) ;
#11183 = EDGE_CURVE ( 'NONE', #17307, #1684, #10010, .T. ) ;
#11184 = LINE ( 'NONE', #20823, #17376 ) ;
#11185 = AXIS2_PLACEMENT_3D ( 'NONE', #18162, #1657, #19437 ) ;
#11186 = ITEM_DEFINED_TRANSFORMATION ( 'NONE', 'NONE', #15744,  #12461 ) ;
#11187 = CARTESIAN_POINT ( 'NONE',  ( 12.54593441764187567, 8.382925368423276069, -13.41830183115846076 ) ) ;
#11188 = EDGE_LOOP ( 'NONE', ( #7449, #10429, #9890, #15166 ) ) ;
#11190 = EDGE_CURVE ( 'NONE', #13652, #10636, #2217, .T. ) ;
#11189 = FACE_OUTER_BOUND ( 'NONE', #16058, .T. ) ;
#11191 = DIRECTION ( 'NONE',  ( -1.000000000000000000, 0.000000000000000000, 0.000000000000000000 ) ) ;
#11192 = ORIENTED_EDGE ( 'NONE', *, *, #8305, .F. ) ;
#11193 = CARTESIAN_POINT ( 'NONE',  ( 2.500000000000000000, -1.178949249685213863, 2.042000000000002924 ) ) ;
#11194 = FACE_OUTER_BOUND ( 'NONE', #13037, .T. ) ;
#11195 = DIRECTION ( 'NONE',  ( 0.000000000000000000, 0.000000000000000000, -1.000000000000000000 ) ) ;
#11196 = CARTESIAN_POINT ( 'NONE',  ( 19.99999999999999645, -27.62776854598897813, 58.65812137498992485 ) ) ;
#11197 = ORIENTED_EDGE ( 'NONE', *, *, #19095, .F. ) ;
#11198 = VECTOR ( 'NONE', #19836, 1000.000000000000114 ) ;
#11199 = FACE_BOUND ( 'NONE', #1980, .T. ) ;
#11200 = CARTESIAN_POINT ( 'NONE',  ( 0.000000000000000000, 0.000000000000000000, 68.00000000000000000 ) ) ;
#11201 = CIRCLE ( 'NONE', #35, 11.49999999999999645 ) ;
#11202 = ORIENTED_EDGE ( 'NONE', *, *, #13366, .T. ) ;
#11203 = CARTESIAN_POINT ( 'NONE',  ( -20.20451054323269346, -11.00838379098076025, -82.59978733170636644 ) ) ;
#11204 = EDGE_CURVE ( 'NONE', #4120, #18964, #9003, .T. ) ;
#11205 = LINE ( 'NONE', #11414, #18826 ) ;
#11206 = CARTESIAN_POINT ( 'NONE',  ( 12.72792205982779379, -12.72792206288790950, -24.54292499981969300 ) ) ;
#11207 = ORIENTED_EDGE ( 'NONE', *, *, #19552, .F. ) ;
#11208 = CARTESIAN_POINT ( 'NONE',  ( 4.248408729364579806, -6.358192988180021210, -10.73864374981968517 ) ) ;
#11209 = ADVANCED_BREP_SHAPE_REPRESENTATION ( '', ( #10194, #12461 ), #8672 ) ;
#11210 = DIRECTION ( 'NONE',  ( -1.000000000000000000, -0.000000000000000000, 0.000000000000000000 ) ) ;
#11211 = DIRECTION ( 'NONE',  ( 1.000000000000000000, 1.836909530733573776E-16, 0.000000000000000000 ) ) ;
#11212 = CARTESIAN_POINT ( 'NONE',  ( 6.888301784570730391, 16.62983158437510411, -16.15863749981969733 ) ) ;
#11213 = CARTESIAN_POINT ( 'NONE',  ( 6.358192988180014993, 4.248408729364578917, 8.915206250180309766 ) ) ;
#11214 = AXIS2_PLACEMENT_3D ( 'NONE', #4668, #18880, #10818 ) ;
#11215 = DIRECTION ( 'NONE',  ( 0.000000000000000000, 0.000000000000000000, 1.000000000000000000 ) ) ;
#11216 = CARTESIAN_POINT ( 'NONE',  ( 13.67243654778934925, 5.663308646854335215, 0.1081455815190729419 ) ) ;
#11217 = EDGE_CURVE ( 'NONE', #2782, #6278, #10786, .T. ) ;
#11218 = DIRECTION ( 'NONE',  ( 0.000000000000000000, 0.000000000000000000, 1.000000000000000000 ) ) ;
#11219 = CIRCLE ( 'NONE', #4109, 72.00000000007199219 ) ;
#11220 = EDGE_LOOP ( 'NONE', ( #20195, #17119 ) ) ;
#11221 = CARTESIAN_POINT ( 'NONE',  ( 19.99999999999999645, 56.42118728228200553, -32.77318456705383198 ) ) ;
#11222 = CYLINDRICAL_SURFACE ( 'NONE', #18171, 80.00000000000000000 ) ;
#11223 = CARTESIAN_POINT ( 'NONE',  ( 30.00000000000000000, -50.00000000000000000, 66.88656633939929463 ) ) ;
#11224 = ORIENTED_EDGE ( 'NONE', *, *, #1202, .F. ) ;
#11225 = AXIS2_PLACEMENT_3D ( 'NONE', #12309, #1304, #11137 ) ;
#11226 = DIRECTION ( 'NONE',  ( 1.000000000000000000, 0.000000000000000000, 0.000000000000000000 ) ) ;
#11227 = VECTOR ( 'NONE', #13643, 1000.000000000000000 ) ;
#11228 = ORIENTED_EDGE ( 'NONE', *, *, #18719, .F. ) ;
#11229 = FACE_OUTER_BOUND ( 'NONE', #19015, .T. ) ;
#11230 = DIRECTION ( 'NONE',  ( 1.000000000000000000, 0.000000000000000000, 0.000000000000000000 ) ) ;
#11231 = ORIENTED_EDGE ( 'NONE', *, *, #9500, .F. ) ;
#11232 = CIRCLE ( 'NONE', #2086, 5.000000000000004441 ) ;
#11233 = ORIENTED_EDGE ( 'NONE', *, *, #18305, .T. ) ;
#11234 = CARTESIAN_POINT ( 'NONE',  ( -6.165580000000000283, 9.267171751443833528E-16, -7.567219999999999835 ) ) ;
#11235 = CARTESIAN_POINT ( 'NONE',  ( 0.000000000000000000, 0.000000000000000000, -130.0000000000000000 ) ) ;
#11236 = CARTESIAN_POINT ( 'NONE',  ( 52.00000000000000000, -39.99999999999999289, 5.000000000000000000 ) ) ;
#11237 = CARTESIAN_POINT ( 'NONE',  ( 4.276731812588570492, -10.32494394809439697, -19.44020274935257220 ) ) ;
#11238 = AXIS2_PLACEMENT_3D ( 'NONE', #9102, #17261, #10895 ) ;
#11239 = CARTESIAN_POINT ( 'NONE',  ( -1.343452921478823292E-09, -11.17563879731704723, 2.301140249713198749 ) ) ;
#11240 = EDGE_CURVE ( 'NONE', #5613, #9780, #10682, .T. ) ;
#11241 = DIRECTION ( 'NONE',  ( 0.000000000000000000, 0.000000000000000000, -1.000000000000000000 ) ) ;
#11242 = CARTESIAN_POINT ( 'NONE',  ( 0.000000000000000000, 0.000000000000000000, 126.0000000000000000 ) ) ;
#11243 = DIRECTION ( 'NONE',  ( 0.000000000000000000, 0.000000000000000000, 1.000000000000000000 ) ) ;
#11244 = ORIENTED_EDGE ( 'NONE', *, *, #20628, .F. ) ;
#11245 = DIRECTION ( 'NONE',  ( -1.000000000000000000, -0.000000000000000000, -0.000000000000000000 ) ) ;
#11246 = ORIENTED_EDGE ( 'NONE', *, *, #9237, .F. ) ;
#11247 = CARTESIAN_POINT ( 'NONE',  ( -16.62983158603122291, -6.888301780572501087, 8.581987500180312978 ) ) ;
#11248 = CARTESIAN_POINT ( 'NONE',  ( 19.99999999999999645, 20.60847369612982405, 61.90898814327722732 ) ) ;
#11249 = VERTEX_POINT ( 'NONE', #13469 ) ;
#11250 = EDGE_CURVE ( 'NONE', #18356, #19780, #2015, .T. ) ;
#11251 = DIRECTION ( 'NONE',  ( 0.000000000000000000, 0.000000000000000000, 1.000000000000000000 ) ) ;
#11252 = ORIENTED_EDGE ( 'NONE', *, *, #12887, .F. ) ;
#11253 = LINE ( 'NONE', #1720, #2741 ) ;
#11254 = CARTESIAN_POINT ( 'NONE',  ( 32.75992285807288340, -31.42540396991885032, 72.63203971126306158 ) ) ;
#11255 = ORIENTED_EDGE ( 'NONE', *, *, #16340, .T. ) ;
#11256 = ORIENTED_EDGE ( 'NONE', *, *, #1629, .F. ) ;
#11257 = LINE ( 'NONE', #7660, #9332 ) ;
#11258 = CIRCLE ( 'NONE', #4823, 2.649999999999999467 ) ;
#11259 = AXIS2_PLACEMENT_3D ( 'NONE', #4008, #10812, #18647 ) ;
#11260 = AXIS2_PLACEMENT_3D ( 'NONE', #3567, #84, #6845 ) ;
#11261 = AXIS2_PLACEMENT_3D ( 'NONE', #12907, #19462, #20729 ) ;
#11262 = DIRECTION ( 'NONE',  ( 1.000000000000000000, -0.000000000000000000, 0.000000000000000000 ) ) ;
#11263 = DIRECTION ( 'NONE',  ( 0.000000000000000000, 1.040834085586084454E-15, -1.000000000000000000 ) ) ;
#11264 = CARTESIAN_POINT ( 'NONE',  ( -7.500000000000000000, 0.000000000000000000, 40.00000000000000000 ) ) ;
#11265 = VECTOR ( 'NONE', #2930, 1000.000000000000000 ) ;
#11266 = ORIENTED_EDGE ( 'NONE', *, *, #16284, .F. ) ;
#11267 = CARTESIAN_POINT ( 'NONE',  ( 21.50000000000000000, 0.000000000000000000, 68.00000000000000000 ) ) ;
#11268 = CARTESIAN_POINT ( 'NONE',  ( 1.491842754445843688, -7.500000000179346316, -0.7245812498196841922 ) ) ;
#11269 = AXIS2_PLACEMENT_3D ( 'NONE', #14707, #19571, #17984 ) ;
#11270 = CARTESIAN_POINT ( 'NONE',  ( 24.99999999999999289, -30.00000000000000711, 44.99999999999998579 ) ) ;
#11271 = DIRECTION ( 'NONE',  ( -1.000000000000000000, 0.000000000000000000, 0.000000000000000000 ) ) ;
#11272 = VECTOR ( 'NONE', #17995, 1000.000000000000000 ) ;
#11273 = EDGE_LOOP ( 'NONE', ( #18084, #599 ) ) ;
#11274 = DIRECTION ( 'NONE',  ( 0.000000000000000000, 0.8169698930104392076, 0.5766803221148710801 ) ) ;
#11275 = CIRCLE ( 'NONE', #16013, 8.999999999999998224 ) ;
#11276 = CARTESIAN_POINT ( 'NONE',  ( -12.50000000000000533, 0.000000000000000000, 43.00000000000000000 ) ) ;
#11277 = CARTESIAN_POINT ( 'NONE',  ( 40.00000000000000711, -40.00000000000001421, -130.0000000000000000 ) ) ;
#11278 = ORIENTED_EDGE ( 'NONE', *, *, #13304, .T. ) ;
#11279 = EDGE_CURVE ( 'NONE', #9969, #16951, #5957, .T. ) ;
#11280 = DIRECTION ( 'NONE',  ( 0.000000000000000000, 0.000000000000000000, 1.000000000000000000 ) ) ;
#11281 = ORIENTED_EDGE ( 'NONE', *, *, #4326, .T. ) ;
#11282 = DIRECTION ( 'NONE',  ( -1.000000000000000000, 0.000000000000000000, 0.000000000000000000 ) ) ;
#11283 = EDGE_CURVE ( 'NONE', #17758, #16351, #18127, .T. ) ;
#11284 = CIRCLE ( 'NONE', #8231, 65.24900000006525147 ) ;
#11285 = EDGE_LOOP ( 'NONE', ( #250, #19985, #19229, #563 ) ) ;
#11286 = EDGE_CURVE ( 'NONE', #12603, #11771, #20514, .T. ) ;
#11287 = DIRECTION ( 'NONE',  ( 0.000000000000000000, 0.9976687691905394839, -0.06824241336466757568 ) ) ;
#11288 = AXIS2_PLACEMENT_3D ( 'NONE', #20054, #9056, #8730 ) ;
#11289 = AXIS2_PLACEMENT_3D ( 'NONE', #4918, #20922, #6708 ) ;
#11290 = CARTESIAN_POINT ( 'NONE',  ( 50.00000000000000000, -124.9999999999999858, 90.00000000000001421 ) ) ;
#11291 = CARTESIAN_POINT ( 'NONE',  ( -1.779019326032424922E-09, -14.79893867758297610, -19.60345808115846111 ) ) ;
#11292 = EDGE_LOOP ( 'NONE', ( #15858, #1201, #15208, #2315 ) ) ;
#11293 = CARTESIAN_POINT ( 'NONE',  ( 7.500000000000000888, 4.207617034106124418E-15, 0.3738000000023073421 ) ) ;
#11294 = PLANE ( 'NONE',  #9912 ) ;
#11295 = ORIENTED_EDGE ( 'NONE', *, *, #18534, .F. ) ;
#11296 = CIRCLE ( 'NONE', #4532, 27.60000000002759890 ) ;
#11297 = CARTESIAN_POINT ( 'NONE',  ( 1.491842754445842578, -7.500000000179340987, -25.83948124981969485 ) ) ;
#11298 = CIRCLE ( 'NONE', #129, 80.00000000000000000 ) ;
#11299 = EDGE_CURVE ( 'NONE', #3180, #10778, #19479, .T. ) ;
#11300 = AXIS2_PLACEMENT_3D ( 'NONE', #4284, #12779, #9159 ) ;
#11301 = CARTESIAN_POINT ( 'NONE',  ( 12.72792206288790950, 12.72792205982780089, 22.13042500018031689 ) ) ;
#11302 = DIRECTION ( 'NONE',  ( -1.000000000000000000, 0.000000000000000000, 0.000000000000000000 ) ) ;
#11303 = LINE ( 'NONE', #2826, #10723 ) ;
#11304 = CIRCLE ( 'NONE', #805, 72.00000000007199219 ) ;
#11305 = VECTOR ( 'NONE', #17619, 1000.000000000000000 ) ;
#11306 = ADVANCED_FACE ( 'NONE', ( #5903 ), #8373, .T. ) ;
#11307 = ORIENTED_EDGE ( 'NONE', *, *, #653, .T. ) ;
#11308 = EDGE_CURVE ( 'NONE', #17074, #14667, #6628, .T. ) ;
#11309 = DIRECTION ( 'NONE',  ( 0.000000000000000000, -1.000000000000000000, -8.673617379884036705E-17 ) ) ;
#11310 =( REPRESENTATION_RELATIONSHIP ('NONE','NONE', #13739, #7225 ) REPRESENTATION_RELATIONSHIP_WITH_TRANSFORMATION ( #15120 )SHAPE_REPRESENTATION_RELATIONSHIP( ) );
#11311 = EDGE_LOOP ( 'NONE', ( #14167, #9119, #15190, #19542 ) ) ;
#11312 = CARTESIAN_POINT ( 'NONE',  ( 62.50000000000000000, -120.0000000000000142, 5.000000000000000000 ) ) ;
#11313 = DIRECTION ( 'NONE',  ( -1.000000000000000000, 0.000000000000000000, 0.000000000000000000 ) ) ;
#11314 = EDGE_CURVE ( 'NONE', #16060, #14491, #19839, .T. ) ;
#11315 = CARTESIAN_POINT ( 'NONE',  ( 6.358192988180019434, 4.248408729364581582, -3.669893749819685969 ) ) ;
#11316 = AXIS2_PLACEMENT_3D ( 'NONE', #3406, #11471, #17846 ) ;
#11317 = ORIENTED_EDGE ( 'NONE', *, *, #17139, .T. ) ;
#11318 = CARTESIAN_POINT ( 'NONE',  ( 19.99999999999999645, -61.72688495901601158, -19.84591825364075746 ) ) ;
#11319 =( NAMED_UNIT ( * ) SI_UNIT ( $, .STERADIAN. ) SOLID_ANGLE_UNIT ( ) );
#11320 = DIRECTION ( 'NONE',  ( -1.000000000000000000, 0.000000000000000000, -0.000000000000000000 ) ) ;
#11321 = DIRECTION ( 'NONE',  ( -0.7935941825507226710, 0.6084474286424838008, -1.131240564625405124E-16 ) ) ;
#11322 = VECTOR ( 'NONE', #5104, 1000.000000000000000 ) ;
#11323 = CARTESIAN_POINT ( 'NONE',  ( -2.163827323447878648E-09, -18.00000000000000355, -21.46019999981969306 ) ) ;
#11324 = ORIENTED_EDGE ( 'NONE', *, *, #19330, .T. ) ;
#11325 = AXIS2_PLACEMENT_3D ( 'NONE', #9139, #2777, #2884 ) ;
#11326 = DIRECTION ( 'NONE',  ( -0.000000000000000000, 0.000000000000000000, 1.000000000000000000 ) ) ;
#11327 = DIRECTION ( 'NONE',  ( -1.508455196501572169E-16, 1.000000000000000000, 0.000000000000000000 ) ) ;
#11328 = EDGE_CURVE ( 'NONE', #8874, #4685, #7481, .T. ) ;
#11329 = CARTESIAN_POINT ( 'NONE',  ( -13.67243654778935102, -5.663308646854334327, -14.02935441848092957 ) ) ;
#11330 = FACE_OUTER_BOUND ( 'NONE', #10563, .T. ) ;
#11331 = VERTEX_POINT ( 'NONE', #14844 ) ;
#11332 = DIRECTION ( 'NONE',  ( 1.000000000000000000, 0.000000000000000000, -0.000000000000000000 ) ) ;
#11333 = EDGE_CURVE ( 'NONE', #14604, #13895, #17838, .T. ) ;
#11334 = CARTESIAN_POINT ( 'NONE',  ( 6.358192988180019434, 4.248408729364581582, 24.60510625018031661 ) ) ;
#11335 = DIRECTION ( 'NONE',  ( -1.000000000000000000, 0.000000000000000000, 0.000000000000000000 ) ) ;
#11336 = VERTEX_POINT ( 'NONE', #18732 ) ;
#11337 = LINE ( 'NONE', #11441, #4482 ) ;
#11338 = VERTEX_POINT ( 'NONE', #8464 ) ;
#11339 = AXIS2_PLACEMENT_3D ( 'NONE', #17457, #20716, #6510 ) ;
#11340 = FACE_BOUND ( 'NONE', #20596, .T. ) ;
#11341 = DIRECTION ( 'NONE',  ( -1.000000000000000000, 0.000000000000000000, 0.000000000000000000 ) ) ;
#11342 = ORIENTED_EDGE ( 'NONE', *, *, #8792, .F. ) ;
#11343 = EDGE_LOOP ( 'NONE', ( #19545, #17433, #15249, #9137, #2900, #6059, #14484, #4564 ) ) ;
#11344 = CARTESIAN_POINT ( 'NONE',  ( 9.999999999999998224, -10.74906464462166866, 71.19310085447965264 ) ) ;
#11345 = EDGE_CURVE ( 'NONE', #701, #17356, #5184, .T. ) ;
#11346 = DIRECTION ( 'NONE',  ( 0.000000000000000000, 0.000000000000000000, 1.000000000000000000 ) ) ;
#11347 = SHAPE_REPRESENTATION_RELATIONSHIP ( 'NONE' , 'NONE' ,  #20346, #6131 ) ;
#11348 = AXIS2_PLACEMENT_3D ( 'NONE', #3357, #16286, #11321 ) ;
#11349 = DIRECTION ( 'NONE',  ( 0.000000000000000000, -1.000000000000000000, 0.000000000000000000 ) ) ;
#11350 = FACE_OUTER_BOUND ( 'NONE', #2226, .T. ) ;
#11351 = CARTESIAN_POINT ( 'NONE',  ( 9.474249097082498849, -6.330490858644140850, -20.32379649935257504 ) ) ;
#11352 = CARTESIAN_POINT ( 'NONE',  ( -11.17563879758427525, -2.222972768810838051, 4.362858999713199459 ) ) ;
#11353 = LINE ( 'NONE', #1514, #16625 ) ;
#11354 = DIRECTION ( 'NONE',  ( 1.000000000000000000, 0.000000000000000000, 0.000000000000000000 ) ) ;
#11355 = CARTESIAN_POINT ( 'NONE',  ( 30.00000000000000000, -30.00000000000000711, 58.09475019311124555 ) ) ;
#11356 = ORIENTED_EDGE ( 'NONE', *, *, #3012, .F. ) ;
#11357 = CYLINDRICAL_SURFACE ( 'NONE', #8530, 8.500000000000000000 ) ;
#11358 = CARTESIAN_POINT ( 'NONE',  ( 3.580422614997668340, 17.99999999956958519, 11.82183125018031511 ) ) ;
#11359 = CARTESIAN_POINT ( 'NONE',  ( 50.00000000000000000, -124.9999999999999858, -90.00000000000001421 ) ) ;
#11360 = ORIENTED_EDGE ( 'NONE', *, *, #12738, .F. ) ;
#11361 = CYLINDRICAL_SURFACE ( 'NONE', #7214, 20.00000000000000355 ) ;
#11362 = ORIENTED_EDGE ( 'NONE', *, *, #4439, .T. ) ;
#11363 = CARTESIAN_POINT ( 'NONE',  ( 0.000000000000000000, 0.000000000000000000, 43.00000000000000000 ) ) ;
#11364 = FACE_OUTER_BOUND ( 'NONE', #18819, .T. ) ;
#11365 = VECTOR ( 'NONE', #14901, 1000.000000000000000 ) ;
#11366 = ORIENTED_EDGE ( 'NONE', *, *, #2050, .T. ) ;
#11367 = ORIENTED_EDGE ( 'NONE', *, *, #17015, .T. ) ;
#11368 = DIRECTION ( 'NONE',  ( -1.000000000000000000, 0.000000000000000000, -0.000000000000000000 ) ) ;
#11369 = EDGE_CURVE ( 'NONE', #5841, #18257, #16629, .T. ) ;
#11370 =( GEOMETRIC_REPRESENTATION_CONTEXT ( 3 ) GLOBAL_UNCERTAINTY_ASSIGNED_CONTEXT ( ( #2213 ) ) GLOBAL_UNIT_ASSIGNED_CONTEXT ( ( #2484, #17109, #9059 ) ) REPRESENTATION_CONTEXT ( 'NONE', 'WORKASPACE' ) );
#11371 = EDGE_CURVE ( 'NONE', #7828, #3309, #9701, .T. ) ;
#11372 = CYLINDRICAL_SURFACE ( 'NONE', #1530, 27.60000000002759890 ) ;
#11373 = DIRECTION ( 'NONE',  ( 1.000000000000000000, 0.000000000000000000, 0.000000000000000000 ) ) ;
#11374 = ORIENTED_EDGE ( 'NONE', *, *, #15850, .F. ) ;
#11375 = CARTESIAN_POINT ( 'NONE',  ( 9.015937996181834148E-10, 7.500000000000000888, 16.86755000018031225 ) ) ;
#11376 = VECTOR ( 'NONE', #1076, 1000.000000000000000 ) ;
#11377 = DIRECTION ( 'NONE',  ( 0.000000000000000000, 0.000000000000000000, 1.000000000000000000 ) ) ;
#11378 = CARTESIAN_POINT ( 'NONE',  ( -65.00002539999999840, 0.000000000000000000, -7.500000000000000000 ) ) ;
#11379 = CARTESIAN_POINT ( 'NONE',  ( 6.249999999999902300, -10.82531754730554496, 46.00000000000000711 ) ) ;
#11380 = CIRCLE ( 'NONE', #10409, 2.649999999999988365 ) ;
#11381 = AXIS2_PLACEMENT_3D ( 'NONE', #10626, #15806, #5947 ) ;
#11382 = EDGE_LOOP ( 'NONE', ( #16864, #15846, #4865, #14890 ) ) ;
#11383 = CYLINDRICAL_SURFACE ( 'NONE', #2754, 20.00000000000000355 ) ;
#11384 = DIRECTION ( 'NONE',  ( -0.000000000000000000, -0.000000000000000000, -1.000000000000000000 ) ) ;
#11385 = LINE ( 'NONE', #19538, #16712 ) ;
#11386 = ORIENTED_EDGE ( 'NONE', *, *, #9885, .T. ) ;
#11387 = DIRECTION ( 'NONE',  ( 0.000000000000000000, 0.000000000000000000, 1.000000000000000000 ) ) ;
#11388 = ORIENTED_EDGE ( 'NONE', *, *, #15535, .F. ) ;
#11389 = CARTESIAN_POINT ( 'NONE',  ( -10.00000000000000000, 0.000000000000000000, 72.00000000007199219 ) ) ;
#11390 = ORIENTED_EDGE ( 'NONE', *, *, #11069, .F. ) ;
#11391 = AXIS2_PLACEMENT_3D ( 'NONE', #20133, #5614, #17188 ) ;
#11392 = DIRECTION ( 'NONE',  ( 1.000000000000000000, 0.000000000000000000, 0.000000000000000000 ) ) ;
#11393 = CIRCLE ( 'NONE', #11723, 17.50000000000000355 ) ;
#11394 = CARTESIAN_POINT ( 'NONE',  ( 7.574999999999881162, -13.12028486733431976, -43.00000000000000000 ) ) ;
#11395 = CARTESIAN_POINT ( 'NONE',  ( -2.222972771497745192, -11.17563879704982632, 19.14339100064742993 ) ) ;
#11396 = ADVANCED_FACE ( 'NONE', ( #18231 ), #11656, .T. ) ;
#11397 = ORIENTED_EDGE ( 'NONE', *, *, #3140, .T. ) ;
#11398 = SURFACE_STYLE_FILL_AREA ( #1755 ) ;
#11399 = DIRECTION ( 'NONE',  ( -1.000000000000000000, -0.000000000000000000, -0.000000000000000000 ) ) ;
#11400 = ORIENTED_EDGE ( 'NONE', *, *, #20764, .T. ) ;
#11401 = CARTESIAN_POINT ( 'NONE',  ( -20.48001470518130773, -6.654962914332837265, -79.70582905289667508 ) ) ;
#11402 = AXIS2_PLACEMENT_3D ( 'NONE', #16523, #3997, #3892 ) ;
#11403 = AXIS2_PLACEMENT_3D ( 'NONE', #5480, #11954, #16836 ) ;
#11404 = CARTESIAN_POINT ( 'NONE',  ( -30.00000000000000000, 36.35083268962917202, 90.00000000000000000 ) ) ;
#11405 = DIRECTION ( 'NONE',  ( 0.000000000000000000, 0.000000000000000000, 1.000000000000000000 ) ) ;
#11406 = CARTESIAN_POINT ( 'NONE',  ( -9.850000000000006750, 0.000000000000000000, -40.00000000000000000 ) ) ;
#11407 = EDGE_CURVE ( 'NONE', #12005, #7112, #9847, .T. ) ;
#11408 = CIRCLE ( 'NONE', #5313, 0.2000000000000000944 ) ;
#11409 = VERTEX_POINT ( 'NONE', #14279 ) ;
#11410 = AXIS2_PLACEMENT_3D ( 'NONE', #9212, #4730, #19350 ) ;
#11411 = CARTESIAN_POINT ( 'NONE',  ( 30.00000000000000711, -40.00000000000001421, -130.0000000000000000 ) ) ;
#11412 = ORIENTED_EDGE ( 'NONE', *, *, #13253, .F. ) ;
#11413 = FACE_OUTER_BOUND ( 'NONE', #19039, .T. ) ;
#11414 = CARTESIAN_POINT ( 'NONE',  ( 19.99999999999999645, -23.08379033237309841, -61.02926039941459635 ) ) ;
#11415 = DIRECTION ( 'NONE',  ( -0.6156453966108028641, 0.000000000000000000, -0.7880233154113698291 ) ) ;
#11416 = B_SPLINE_CURVE_WITH_KNOTS ( 'NONE', 3,
 ( #17907, #3367, #9832, #8141, #19377, #20862, #12831, #9742, #13139, #19586, #1789, #8245, #11523, #17997, #4756, #9936, #8350, #1694, #14828, #12726, #4663, #11223 ),
 .UNSPECIFIED., .F., .F.,
 ( 4, 2, 2, 2, 2, 2, 2, 2, 2, 2, 4 ),
 ( 0.008203449124722041533, 0.01993989471859326790, 0.02287400611706106451, 0.02580811751552886807, 0.03167634031246444049, 0.03461045171093222322, 0.03754456310939999902, 0.04341278590633557144, 0.04928100870327114386, 0.05221512010173892659, 0.05514923150020671627 ),
 .UNSPECIFIED. ) ;
#11417 = AXIS2_PLACEMENT_3D ( 'NONE', #6440, #9644, #16106 ) ;
#11418 = ORIENTED_EDGE ( 'NONE', *, *, #7392, .T. ) ;
#11419 = CARTESIAN_POINT ( 'NONE',  ( 30.00000000000000000, -170.8299878242309546, -15.48896927112552824 ) ) ;
#11420 = VECTOR ( 'NONE', #1270, 1000.000000000000000 ) ;
#11421 = DIRECTION ( 'NONE',  ( 1.000000000000000000, 0.000000000000000000, 0.000000000000000000 ) ) ;
#11422 =( NAMED_UNIT ( * ) PLANE_ANGLE_UNIT ( ) SI_UNIT ( $, .RADIAN. ) );
#11423 = CARTESIAN_POINT ( 'NONE',  ( 3.580422610670021211, -18.00000000043041481, -21.75473124981969164 ) ) ;
#11424 = EDGE_CURVE ( 'NONE', #17144, #5709, #15756, .T. ) ;
#11426 = ORIENTED_EDGE ( 'NONE', *, *, #19926, .F. ) ;
#11425 = VECTOR ( 'NONE', #14095, 1000.000000000000000 ) ;
#11427 = AXIS2_PLACEMENT_3D ( 'NONE', #4390, #17753, #6295 ) ;
#11428 = EDGE_CURVE ( 'NONE', #15524, #18653, #9022, .T. ) ;
#11429 = CARTESIAN_POINT ( 'NONE',  ( 4.248408730893246776, 6.358192987158592047, 8.326143750180307279 ) ) ;
#11430 = FACE_BOUND ( 'NONE', #5977, .T. ) ;
#11431 = CARTESIAN_POINT ( 'NONE',  ( 1.779017513685135741E-09, 14.79893867758296544, -11.08404191848092779 ) ) ;
#11432 = DIRECTION ( 'NONE',  ( -0.000000000000000000, -1.000000000000000000, -0.000000000000000000 ) ) ;
#11433 = ADVANCED_FACE ( 'NONE', ( #19251 ), #1257, .T. ) ;
#11434 = AXIS2_PLACEMENT_3D ( 'NONE', #6419, #12810, #1950 ) ;
#11435 = ORIENTED_EDGE ( 'NONE', *, *, #14701, .F. ) ;
#11436 = CARTESIAN_POINT ( 'NONE',  ( 9.999999999999998224, -53.26727847779503833, -48.44168704307686113 ) ) ;
#11437 = VECTOR ( 'NONE', #19242, 1000.000000000000000 ) ;
#11438 = DIRECTION ( 'NONE',  ( 1.000000000000000000, -0.000000000000000000, 0.000000000000000000 ) ) ;
#11439 = DIRECTION ( 'NONE',  ( 0.000000000000000000, -1.000000000000000000, 0.000000000000000000 ) ) ;
#11440 = ORIENTED_EDGE ( 'NONE', *, *, #6122, .T. ) ;
#11441 = CARTESIAN_POINT ( 'NONE',  ( 50.00000000000000000, 230.0000000000000000, 84.99999999999998579 ) ) ;
#11442 = CIRCLE ( 'NONE', #17879, 65.24900000006525147 ) ;
#11443 = VERTEX_POINT ( 'NONE', #3039 ) ;
#11444 = FACE_OUTER_BOUND ( 'NONE', #16829, .T. ) ;
#11445 = DIRECTION ( 'NONE',  ( 0.000000000000000000, 0.000000000000000000, -1.000000000000000000 ) ) ;
#11446 = ORIENTED_EDGE ( 'NONE', *, *, #17982, .T. ) ;
#11447 = EDGE_CURVE ( 'NONE', #4931, #18682, #17669, .T. ) ;
#11448 = ORIENTED_EDGE ( 'NONE', *, *, #4433, .T. ) ;
#11449 = CARTESIAN_POINT ( 'NONE',  ( 0.000000000000000000, 0.000000000000000000, 0.000000000000000000 ) ) ;
#11450 = EDGE_CURVE ( 'NONE', #8987, #44, #9609, .T. ) ;
#11451 = DIRECTION ( 'NONE',  ( -0.000000000000000000, -0.000000000000000000, 1.000000000000000000 ) ) ;
#11452 = CYLINDRICAL_SURFACE ( 'NONE', #3837, 2.649999999999994582 ) ;
#11453 = EDGE_CURVE ( 'NONE', #16334, #16803, #15647, .T. ) ;
#11454 = SURFACE_STYLE_FILL_AREA ( #14120 ) ;
#11455 = CARTESIAN_POINT ( 'NONE',  ( 4.248408729364579806, -6.358192988180021210, 17.53635625018031519 ) ) ;
#11456 = CARTESIAN_POINT ( 'NONE',  ( 4.276731815070940357, 10.32494394706615815, 7.602702749713199815 ) ) ;
#11457 = DIRECTION ( 'NONE',  ( 1.000000000000000000, 0.000000000000000000, 0.000000000000000000 ) ) ;
#11458 = CYLINDRICAL_SURFACE ( 'NONE', #10345, 7.500000000000000000 ) ;
#11459 = ORIENTED_EDGE ( 'NONE', *, *, #16212, .T. ) ;
#11460 = CARTESIAN_POINT ( 'NONE',  ( 19.99999999999999645, 0.000000000000000000, 0.000000000000000000 ) ) ;
#11461 = CARTESIAN_POINT ( 'NONE',  ( 10.19618095047497874, -15.25966317163203279, 5.931206250180311557 ) ) ;
#11462 = CARTESIAN_POINT ( 'NONE',  ( 19.99999999999999645, 63.85430960833490843, -11.25592921604860663 ) ) ;
#11463 = ORIENTED_EDGE ( 'NONE', *, *, #10103, .T. ) ;
#11464 = DIRECTION ( 'NONE',  ( -1.000000000000000000, 0.000000000000000000, 0.000000000000000000 ) ) ;
#11465 = VERTEX_POINT ( 'NONE', #11100 ) ;
#11466 = CARTESIAN_POINT ( 'NONE',  ( 0.000000000000000000, -29.55812890832026341, 65.65300461859676773 ) ) ;
#11467 = CARTESIAN_POINT ( 'NONE',  ( 33.23318211478949991, -29.69549557693871833, -67.81563648932102240 ) ) ;
#11468 = VERTEX_POINT ( 'NONE', #9186 ) ;
#11469 = ORIENTED_EDGE ( 'NONE', *, *, #13687, .F. ) ;
#11470 = CARTESIAN_POINT ( 'NONE',  ( 2.500000000000002220, 0.000000000000000000, -25.03750572909317285 ) ) ;
#11471 = DIRECTION ( 'NONE',  ( 1.000000000000000000, -0.000000000000000000, -0.000000000000000000 ) ) ;
#11472 = DIRECTION ( 'NONE',  ( -1.000000000000000000, 0.000000000000000000, 0.000000000000000000 ) ) ;
#11473 = ORIENTED_EDGE ( 'NONE', *, *, #5336, .F. ) ;
#11474 = CARTESIAN_POINT ( 'NONE',  ( -5.303300859536631329, -5.303300858261583706, 3.908175000180312164 ) ) ;
#11475 = DIRECTION ( 'NONE',  ( -1.000000000000000000, 0.000000000000000000, -0.000000000000000000 ) ) ;
#11476 = FACE_OUTER_BOUND ( 'NONE', #8522, .T. ) ;
#11477 = CARTESIAN_POINT ( 'NONE',  ( 19.99999999999999645, 64.52323195238639642, -6.389157729492497495 ) ) ;
#11478 = EDGE_LOOP ( 'NONE', ( #4977, #1961 ) ) ;
#11479 = EDGE_CURVE ( 'NONE', #9276, #19491, #14116, .T. ) ;
#11480 = CARTESIAN_POINT ( 'NONE',  ( 0.000000000000000000, 0.000000000000000000, 0.000000000000000000 ) ) ;
#11481 = ORIENTED_EDGE ( 'NONE', *, *, #7210, .T. ) ;
#11482 = CARTESIAN_POINT ( 'NONE',  ( 3.580422610670020322, -18.00000000043041126, 14.04066875018031446 ) ) ;
#11483 = DIRECTION ( 'NONE',  ( -1.000000000000000000, 0.000000000000000000, 0.000000000000000000 ) ) ;
#11484 = ORIENTED_EDGE ( 'NONE', *, *, #2742, .T. ) ;
#11485 = PLANE ( 'NONE',  #2815 ) ;
#11486 = ORIENTED_EDGE ( 'NONE', *, *, #11013, .F. ) ;
#11487 = DIRECTION ( 'NONE',  ( -1.000000000000000000, -0.000000000000000000, -0.000000000000000000 ) ) ;
#11488 = VERTEX_POINT ( 'NONE', #7597 ) ;
#11489 = CARTESIAN_POINT ( 'NONE',  ( 19.99999999999999645, -51.43306257653114955, -40.15061736769617795 ) ) ;
#11490 = CARTESIAN_POINT ( 'NONE',  ( -10.00000000000000000, 0.000000000000000000, 0.000000000000000000 ) ) ;
#11491 = CARTESIAN_POINT ( 'NONE',  ( 5.663308646854342321, -13.67243654778935635, -20.19252058115845827 ) ) ;
#11492 = ORIENTED_EDGE ( 'NONE', *, *, #14253, .F. ) ;
#11493 = DIRECTION ( 'NONE',  ( 0.000000000000000000, 0.9790840876823220240, 0.2034560130526375243 ) ) ;
#11494 = DIRECTION ( 'NONE',  ( 0.000000000000000000, 0.8660254037844380415, -0.5000000000000009992 ) ) ;
#11495 = ORIENTED_EDGE ( 'NONE', *, *, #808, .F. ) ;
#11496 = CARTESIAN_POINT ( 'NONE',  ( -1.318516776095821186, -3.857556137907092175, -1.739862437281285109E-14 ) ) ;
#11497 = EDGE_CURVE ( 'NONE', #1320, #8003, #12053, .T. ) ;
#11498 = CARTESIAN_POINT ( 'NONE',  ( 30.00000000000000355, -139.6410161513775563, -90.00000000000001421 ) ) ;
#11499 = DIRECTION ( 'NONE',  ( 0.000000000000000000, 0.000000000000000000, 1.000000000000000000 ) ) ;
#11500 = DIRECTION ( 'NONE',  ( -1.000000000000000000, 0.000000000000000000, 0.000000000000000000 ) ) ;
#11501 = ORIENTED_EDGE ( 'NONE', *, *, #10612, .F. ) ;
#11502 = CARTESIAN_POINT ( 'NONE',  ( -4.000000000000000000, 2.309401076758496263, -0.3572655899081631503 ) ) ;
#11503 = ORIENTED_EDGE ( 'NONE', *, *, #9111, .F. ) ;
#11504 = EDGE_CURVE ( 'NONE', #13626, #1069, #2924, .T. ) ;
#11505 = PRESENTATION_STYLE_ASSIGNMENT (( #14700 ) ) ;
#11506 = CYLINDRICAL_SURFACE ( 'NONE', #12737, 65.24900000006525147 ) ;
#11507 = COLOUR_RGB ( '', 0.66274510, 0.83137255, 0.94901961) ;
#11508 = ORIENTED_EDGE ( 'NONE', *, *, #10249, .F. ) ;
#11509 = FACE_OUTER_BOUND ( 'NONE', #20284, .T. ) ;
#11510 = CYLINDRICAL_SURFACE ( 'NONE', #19722, 2.649999999999999467 ) ;
#11511 = PRODUCT_CONTEXT ( 'NONE', #11824, 'mechanical' ) ;
#11512 = CARTESIAN_POINT ( 'NONE',  ( -17.99999999956958874, 3.580422614997675002, -18.80941874981969164 ) ) ;
#11513 = VERTEX_POINT ( 'NONE', #2936 ) ;
#11514 = VECTOR ( 'NONE', #10539, 1000.000000000000000 ) ;
#11515 = DIRECTION ( 'NONE',  ( -1.000000000000000000, 0.000000000000000000, 0.000000000000000000 ) ) ;
#11516 =( LENGTH_UNIT ( ) NAMED_UNIT ( * ) SI_UNIT ( .MILLI., .METRE. ) );
#11517 = CARTESIAN_POINT ( 'NONE',  ( -14.79893867793683349, -2.943691925285398359, -4.309823168480927613 ) ) ;
#11518 = PLANE ( 'NONE',  #4827 ) ;
#11519 = AXIS2_PLACEMENT_3D ( 'NONE', #19943, #7335, #13501 ) ;
#11520 = ORIENTED_EDGE ( 'NONE', *, *, #11968, .F. ) ;
#11521 = CARTESIAN_POINT ( 'NONE',  ( 19.99999999999999645, 51.43306257653143376, 40.15061736769582268 ) ) ;
#11522 = CARTESIAN_POINT ( 'NONE',  ( 16.55500000000001393, 3.061616997868383634E-16, -2.500000000000000444 ) ) ;
#11523 = CARTESIAN_POINT ( 'NONE',  ( 32.70638587058282098, -31.60219482138385061, 67.47980676442061565 ) ) ;
#11524 = ORIENTED_EDGE ( 'NONE', *, *, #1261, .F. ) ;
#11525 = ADVANCED_FACE ( 'NONE', ( #17571 ), #4522, .F. ) ;
#11526 = CARTESIAN_POINT ( 'NONE',  ( 19.99999999999999645, -29.55812890832025985, 65.65300461859676773 ) ) ;
#11527 = ORIENTED_EDGE ( 'NONE', *, *, #380, .F. ) ;
#11528 = LINE ( 'NONE', #11844, #15291 ) ;
#11529 = CARTESIAN_POINT ( 'NONE',  ( 50.00000000000000000, 230.0000000000000000, 0.000000000000000000 ) ) ;
#11530 = EDGE_CURVE ( 'NONE', #12115, #18900, #1145, .T. ) ;
#11531 = AXIS2_PLACEMENT_3D ( 'NONE', #2275, #12020, #15201 ) ;
#11532 = EDGE_LOOP ( 'NONE', ( #16454, #7326, #13455, #19051 ) ) ;
#11533 = ORIENTED_EDGE ( 'NONE', *, *, #548, .T. ) ;
#11534 = CARTESIAN_POINT ( 'NONE',  ( 45.73369142091321748, -8.073147882754625471, 78.54250490773422655 ) ) ;
#11535 = ADVANCED_FACE ( 'NONE', ( #1461 ), #3588, .T. ) ;
#11536 = DIRECTION ( 'NONE',  ( -1.000000000000000000, 0.000000000000000000, 0.000000000000000000 ) ) ;
#11537 = CIRCLE ( 'NONE', #4782, 2.649999999999993694 ) ;
#11538 = EDGE_CURVE ( 'NONE', #9241, #11681, #16806, .T. ) ;
#11539 = CARTESIAN_POINT ( 'NONE',  ( 19.99999999999999645, 0.000000000000000000, 0.000000000000000000 ) ) ;
#11540 = PRODUCT_RELATED_PRODUCT_CATEGORY ( 'part', '', ( #7468 ) ) ;
#11541 = CYLINDRICAL_SURFACE ( 'NONE', #19345, 8.999999999999998224 ) ;
#11542 = CARTESIAN_POINT ( 'NONE',  ( -6.358192988180021210, -4.248408729364580694, 10.46760625018031376 ) ) ;
#11543 = CARTESIAN_POINT ( 'NONE',  ( -2.222972768810836275, 11.17563879758427525, -2.705891000286804182 ) ) ;
#11544 = CARTESIAN_POINT ( 'NONE',  ( 2.500000000000000000, 2.357898499370433054, -1.951563910473907981E-15 ) ) ;
#11545 = LINE ( 'NONE', #6674, #2909 ) ;
#11546 = AXIS2_PLACEMENT_3D ( 'NONE', #7076, #13555, #20225 ) ;
#11547 = EDGE_CURVE ( 'NONE', #11144, #17642, #11303, .T. ) ;
#11548 = CONICAL_SURFACE ( 'NONE', #9528, 2.041999999999999815, 1.047197551196591858 ) ;
#11549 = ORIENTED_EDGE ( 'NONE', *, *, #482, .F. ) ;
#11550 = DIRECTION ( 'NONE',  ( 1.000000000000000000, 0.000000000000000000, 0.000000000000000000 ) ) ;
#11551 = CARTESIAN_POINT ( 'NONE',  ( -10.19618095414378622, -15.25966316918061416, 17.12339375018031262 ) ) ;
#11552 = PLANE ( 'NONE',  #5915 ) ;
#11553 = AXIS2_PLACEMENT_3D ( 'NONE', #15035, #13546, #5688 ) ;
#11554 = VERTEX_POINT ( 'NONE', #20526 ) ;
#11555 = EDGE_CURVE ( 'NONE', #13182, #11249, #4946, .T. ) ;
#11556 = CYLINDRICAL_SURFACE ( 'NONE', #2828, 65.24900000006525147 ) ;
#11557 = VERTEX_POINT ( 'NONE', #20625 ) ;
#11558 = DIRECTION ( 'NONE',  ( -1.000000000000000000, -0.000000000000000000, -0.000000000000000000 ) ) ;
#11559 = CARTESIAN_POINT ( 'NONE',  ( 30.75237355671447048, -40.04063416367457506, 71.40923356276123002 ) ) ;
#11560 = ADVANCED_FACE ( 'NONE', ( #6103 ), #10987, .T. ) ;
#11561 = ORIENTED_EDGE ( 'NONE', *, *, #16113, .T. ) ;
#11562 = MECHANICAL_DESIGN_GEOMETRIC_PRESENTATION_REPRESENTATION (  '', ( #20343 ), #10554 ) ;
#11563 = ORIENTED_EDGE ( 'NONE', *, *, #15706, .T. ) ;
#11564 = LINE ( 'NONE', #16437, #12409 ) ;
#11565 = ADVANCED_FACE ( 'NONE', ( #5248 ), #490, .T. ) ;
#11566 = DIRECTION ( 'NONE',  ( 0.000000000000000000, 0.000000000000000000, 1.000000000000000000 ) ) ;
#11567 = AXIS2_PLACEMENT_3D ( 'NONE', #9483, #1239, #1551 ) ;
#11568 = VECTOR ( 'NONE', #4036, 1000.000000000000000 ) ;
#11569 = DIRECTION ( 'NONE',  ( -1.000000000000000000, -0.000000000000000000, -0.000000000000000000 ) ) ;
#11570 = AXIS2_PLACEMENT_3D ( 'NONE', #7412, #15574, #969 ) ;
#11571 = ORIENTED_EDGE ( 'NONE', *, *, #19482, .F. ) ;
#11572 = CARTESIAN_POINT ( 'NONE',  ( -9.015947181032828388E-10, -7.500000000000000888, 12.15505000018031367 ) ) ;
#11573 = CARTESIAN_POINT ( 'NONE',  ( 31.02182833614992674, -111.3267134195865395, -79.49107265470053107 ) ) ;
#11574 = DIRECTION ( 'NONE',  ( 0.000000000000000000, -1.000000000000000000, 0.000000000000000000 ) ) ;
#11575 = CARTESIAN_POINT ( 'NONE',  ( 30.00000000000000000, -99.99999999999998579, 52.00000000000000000 ) ) ;
#11576 = FACE_OUTER_BOUND ( 'NONE', #13685, .T. ) ;
#11577 = ADVANCED_FACE ( 'NONE', ( #15002 ), #16380, .T. ) ;
#11578 = ORIENTED_EDGE ( 'NONE', *, *, #4679, .T. ) ;
#11579 = CARTESIAN_POINT ( 'NONE',  ( 2.500000000000000000, -1.178949249685214307, 2.042000000000001592 ) ) ;
#11580 = ORIENTED_EDGE ( 'NONE', *, *, #11345, .T. ) ;
#11581 = CARTESIAN_POINT ( 'NONE',  ( -12.50000000000000533, 0.000000000000000000, 126.0000000000000000 ) ) ;
#11582 = DIRECTION ( 'NONE',  ( 0.000000000000000000, 0.000000000000000000, 1.000000000000000000 ) ) ;
#11583 = CIRCLE ( 'NONE', #7869, 27.60000000002759890 ) ;
#11584 = EDGE_LOOP ( 'NONE', ( #2206, #12354 ) ) ;
#11585 = AXIS2_PLACEMENT_3D ( 'NONE', #11659, #8780, #13255 ) ;
#11586 = FACE_OUTER_BOUND ( 'NONE', #9019, .T. ) ;
#11587 = VERTEX_POINT ( 'NONE', #371 ) ;
#11588 = CARTESIAN_POINT ( 'NONE',  ( 20.55500000000001748, 3.061616997868384127E-16, -2.500000000000000888 ) ) ;
#11589 = FACE_OUTER_BOUND ( 'NONE', #13225, .T. ) ;
#11590 = AXIS2_PLACEMENT_3D ( 'NONE', #3468, #18214, #10152 ) ;
#11591 = ORIENTED_EDGE ( 'NONE', *, *, #14468, .T. ) ;
#11592 = AXIS2_PLACEMENT_3D ( 'NONE', #13438, #12044, #11931 ) ;
#11593 = DIRECTION ( 'NONE',  ( 1.000000000000000000, -0.000000000000000000, -0.000000000000000000 ) ) ;
#11594 = EDGE_CURVE ( 'NONE', #1369, #141, #5286, .T. ) ;
#11595 = CARTESIAN_POINT ( 'NONE',  ( 0.000000000000000000, -18.50424539729797502, -69.58155576219135696 ) ) ;
#11596 = CARTESIAN_POINT ( 'NONE',  ( 2.222972771497741640, 11.17563879704982988, 5.005891000647428868 ) ) ;
#11597 = CIRCLE ( 'NONE', #1469, 72.00000000007199219 ) ;
#11599 = ORIENTED_EDGE ( 'NONE', *, *, #10240, .T. ) ;
#11598 = AXIS2_PLACEMENT_3D ( 'NONE', #16297, #12029, #4065 ) ;
#11600 = PRESENTATION_STYLE_ASSIGNMENT (( #3434 ) ) ;
#11601 = AXIS2_PLACEMENT_3D ( 'NONE', #8673, #16527, #13356 ) ;
#11602 = DIRECTION ( 'NONE',  ( 0.000000000000000000, 0.2697967711570248839, -0.9629172873477991335 ) ) ;
#11603 = ORIENTED_EDGE ( 'NONE', *, *, #109, .T. ) ;
#11604 = DIRECTION ( 'NONE',  ( 0.000000000000000000, 1.000000000000000000, 0.000000000000000000 ) ) ;
#11605 = ORIENTED_EDGE ( 'NONE', *, *, #11908, .F. ) ;
#11606 = CARTESIAN_POINT ( 'NONE',  ( -18.00000000043041126, -3.580422610670022099, 18.30151875018031760 ) ) ;
#11607 = DIRECTION ( 'NONE',  ( 1.000000000000000000, 0.000000000000000000, 0.000000000000000000 ) ) ;
#11608 = DIRECTION ( 'NONE',  ( -1.000000000000000000, 0.000000000000000000, 0.000000000000000000 ) ) ;
#11609 = VECTOR ( 'NONE', #9064, 1000.000000000000000 ) ;
#11610 = ORIENTED_EDGE ( 'NONE', *, *, #8959, .T. ) ;
#11611 = DIRECTION ( 'NONE',  ( -1.000000000000000000, 0.000000000000000000, 0.000000000000000000 ) ) ;
#11612 = ORIENTED_EDGE ( 'NONE', *, *, #14429, .T. ) ;
#11613 = AXIS2_PLACEMENT_3D ( 'NONE', #19635, #1744, #6599 ) ;
#11614 = DIRECTION ( 'NONE',  ( 0.000000000000000000, 0.000000000000000000, -1.000000000000000000 ) ) ;
#11615 = ORIENTED_EDGE ( 'NONE', *, *, #7252, .F. ) ;
#11616 = DIRECTION ( 'NONE',  ( 0.000000000000000000, 0.000000000000000000, 1.000000000000000000 ) ) ;
#11617 = EDGE_CURVE ( 'NONE', #11587, #14616, #5349, .T. ) ;
#11618 = DIRECTION ( 'NONE',  ( 0.000000000000000000, -0.9422609221188236184, 0.3348796121709771145 ) ) ;
#11619 = SHAPE_DEFINITION_REPRESENTATION ( #18831, #3036 ) ;
#11620 = VECTOR ( 'NONE', #11415, 1000.000000000000000 ) ;
#11621 = CARTESIAN_POINT ( 'NONE',  ( -8.382925368423274293, 12.54593441764187745, 21.92544816884154457 ) ) ;
#11622 = VERTEX_POINT ( 'NONE', #16183 ) ;
#11623 = DIRECTION ( 'NONE',  ( 0.000000000000000000, 0.000000000000000000, 1.000000000000000000 ) ) ;
#11624 = VECTOR ( 'NONE', #3614, 1000.000000000000000 ) ;
#11625 = CYLINDRICAL_SURFACE ( 'NONE', #609, 2.500000000000000444 ) ;
#11626 = CIRCLE ( 'NONE', #3842, 65.24900000006526568 ) ;
#11627 = CARTESIAN_POINT ( 'NONE',  ( 14.79893867722909917, -2.943691928843437111, 0.9917393315190744518 ) ) ;
#11628 = CARTESIAN_POINT ( 'NONE',  ( 3.678949249685231848, 5.299604027854762026E-17, 0.000000000000000000 ) ) ;
#11629 = ORIENTED_EDGE ( 'NONE', *, *, #12963, .F. ) ;
#11630 = CARTESIAN_POINT ( 'NONE',  ( 3.600000000000054712, 10.82531754730546147, 43.00000000000000000 ) ) ;
#11631 = CYLINDRICAL_SURFACE ( 'NONE', #11736, 10.85999999999999410 ) ;
#11632 = CARTESIAN_POINT ( 'NONE',  ( 2.500000000000000000, -1.178949249685214307, 2.042000000000001592 ) ) ;
#11633 = CIRCLE ( 'NONE', #17043, 27.60000000002759890 ) ;
#11634 = ORIENTED_EDGE ( 'NONE', *, *, #16875, .F. ) ;
#11635 = CIRCLE ( 'NONE', #814, 65.24900000006525147 ) ;
#11636 = CARTESIAN_POINT ( 'NONE',  ( 19.99999999999999645, -51.43306257653170377, 40.15061736769546741 ) ) ;
#11637 = VERTEX_POINT ( 'NONE', #14797 ) ;
#11638 = DIRECTION ( 'NONE',  ( 0.000000000000000000, 0.000000000000000000, 1.000000000000000000 ) ) ;
#11639 = CARTESIAN_POINT ( 'NONE',  ( 30.00000000000000355, -139.6410161513775563, -85.00000000000000000 ) ) ;
#11640 = ORIENTED_EDGE ( 'NONE', *, *, #18263, .T. ) ;
#11641 = ORIENTED_EDGE ( 'NONE', *, *, #18044, .F. ) ;
#11642 = DIRECTION ( 'NONE',  ( 0.000000000000000000, 0.5000000000000011102, 0.8660254037844379305 ) ) ;
#11643 = AXIS2_PLACEMENT_3D ( 'NONE', #7002, #755, #8596 ) ;
#11644 = CIRCLE ( 'NONE', #18412, 2.649999999999987477 ) ;
#11645 = CARTESIAN_POINT ( 'NONE',  ( 24.99999999999999645, -85.00000000000000000, 75.00000000000000000 ) ) ;
#11646 = DIRECTION ( 'NONE',  ( -0.000000000000000000, -0.000000000000000000, 1.000000000000000000 ) ) ;
#11647 = FILL_AREA_STYLE_COLOUR ( '', #1540 ) ;
#11648 = CARTESIAN_POINT ( 'NONE',  ( 21.50000000000000000, 0.000000000000000000, 84.99999999999998579 ) ) ;
#11649 = DIRECTION ( 'NONE',  ( 0.000000000000000000, 0.000000000000000000, 1.000000000000000000 ) ) ;
#11650 = CARTESIAN_POINT ( 'NONE',  ( -6.358192988180021210, -4.248408729364580694, 19.89260625018031803 ) ) ;
#11651 = AXIS2_PLACEMENT_3D ( 'NONE', #11899, #10212, #20160 ) ;
#11652 = ADVANCED_FACE ( 'NONE', ( #6618 ), #1590, .F. ) ;
#11653 = CARTESIAN_POINT ( 'NONE',  ( -6.330490856366290053, 9.474249098604506258, 6.130046499713198926 ) ) ;
#11654 = EDGE_CURVE ( 'NONE', #9981, #588, #14694, .T. ) ;
#11655 = CARTESIAN_POINT ( 'NONE',  ( 6.250000000000054179, 10.82531754730546147, 43.00000000000000000 ) ) ;
#11656 = CYLINDRICAL_SURFACE ( 'NONE', #9355, 65.24900000006525147 ) ;
#11657 = AXIS2_PLACEMENT_3D ( 'NONE', #4011, #6882, #11864 ) ;
#11658 = EDGE_LOOP ( 'NONE', ( #20898, #11197, #20460, #683 ) ) ;
#11659 = CARTESIAN_POINT ( 'NONE',  ( 6.999999999999999112, 7.118024431592597790E-15, 0.000000000000000000 ) ) ;
#11660 = CARTESIAN_POINT ( 'NONE',  ( -6.888301780572501976, 16.62983158603122291, 10.93823750018031404 ) ) ;
#11661 = DIRECTION ( 'NONE',  ( 0.000000000000000000, 0.000000000000000000, 1.000000000000000000 ) ) ;
#11662 = EDGE_CURVE ( 'NONE', #10684, #5273, #13752, .T. ) ;
#11663 = ORIENTED_EDGE ( 'NONE', *, *, #20584, .F. ) ;
#11664 = DIRECTION ( 'NONE',  ( 1.000000000000000000, 0.000000000000000000, 0.000000000000000000 ) ) ;
#11665 = EDGE_LOOP ( 'NONE', ( #11953, #1137, #2861, #9715 ) ) ;
#11666 = LINE ( 'NONE', #5001, #9860 ) ;
#11667 = DIRECTION ( 'NONE',  ( 1.000000000000000000, -0.000000000000000000, -0.000000000000000000 ) ) ;
#11668 = ORIENTED_EDGE ( 'NONE', *, *, #8747, .F. ) ;
#11669 = ORIENTED_EDGE ( 'NONE', *, *, #12307, .T. ) ;
#11670 =( GEOMETRIC_REPRESENTATION_CONTEXT ( 3 ) GLOBAL_UNCERTAINTY_ASSIGNED_CONTEXT ( ( #5384 ) ) GLOBAL_UNIT_ASSIGNED_CONTEXT ( ( #6360, #4567, #6453 ) ) REPRESENTATION_CONTEXT ( 'NONE', 'WORKASPACE' ) );
#11671 = DIRECTION ( 'NONE',  ( 0.000000000000000000, 0.000000000000000000, 1.000000000000000000 ) ) ;
#11672 = DIRECTION ( 'NONE',  ( 0.000000000000000000, 0.000000000000000000, 1.000000000000000000 ) ) ;
#11673 = ADVANCED_FACE ( 'NONE', ( #3547 ), #898, .F. ) ;
#11674 = CIRCLE ( 'NONE', #17789, 65.24900000006525147 ) ;
#11675 = CARTESIAN_POINT ( 'NONE',  ( 8.899999999999890221, -10.82531754730554496, 46.00000000000000711 ) ) ;
#11676 = EDGE_CURVE ( 'NONE', #2302, #10641, #10020, .T. ) ;
#11677 = CARTESIAN_POINT ( 'NONE',  ( -7.499999999820661678, 1.491842756249031288, 5.380831250180311720 ) ) ;
#11678 = EDGE_CURVE ( 'NONE', #2494, #9919, #18153, .T. ) ;
#11679 = CARTESIAN_POINT ( 'NONE',  ( 38.54445100392999990, -121.4157858342328495, -86.08560793638669395 ) ) ;
#11680 = CARTESIAN_POINT ( 'NONE',  ( 5.000000000000002665, 3.306546357697854226E-16, 2.700000000000000622 ) ) ;
#11681 = VERTEX_POINT ( 'NONE', #11833 ) ;
#11682 = DIRECTION ( 'NONE',  ( 1.000000000000000000, 0.000000000000000000, 0.000000000000000000 ) ) ;
#11683 = DIRECTION ( 'NONE',  ( 0.000000000000000000, 0.000000000000000000, 1.000000000000000000 ) ) ;
#11684 = ORIENTED_EDGE ( 'NONE', *, *, #20429, .F. ) ;
#11685 = CARTESIAN_POINT ( 'NONE',  ( 19.99999999999999645, 0.000000000000000000, 0.000000000000000000 ) ) ;
#11686 = ORIENTED_EDGE ( 'NONE', *, *, #1714, .F. ) ;
#11687 = ADVANCED_FACE ( 'NONE', ( #19874 ), #8422, .T. ) ;
#11688 = CARTESIAN_POINT ( 'NONE',  ( 10.19618095047497874, -15.25966317163203279, 13.45160625018031553 ) ) ;
#11689 = DIRECTION ( 'NONE',  ( -0.000000000000000000, -0.000000000000000000, -1.000000000000000000 ) ) ;
#11690 = ORIENTED_EDGE ( 'NONE', *, *, #1838, .T. ) ;
#11691 = LINE ( 'NONE', #16560, #14008 ) ;
#11692 = ORIENTED_EDGE ( 'NONE', *, *, #14449, .T. ) ;
#11693 = AXIS2_PLACEMENT_3D ( 'NONE', #13720, #13610, #20059 ) ;
#11694 = PRODUCT_DEFINITION_SHAPE ( 'NONE', 'NONE',  #20951 ) ;
#11695 = CARTESIAN_POINT ( 'NONE',  ( 0.000000000000000000, 0.000000000000000000, 0.000000000000000000 ) ) ;
#11696 = DIRECTION ( 'NONE',  ( 0.000000000000000000, 0.000000000000000000, -1.000000000000000000 ) ) ;
#11697 =( BOUNDED_SURFACE ( )  B_SPLINE_SURFACE ( 1, 2, ( 
 ( #11791, #5109, #18254, #17859, #16159, #1942, #14668, #8400, #346, #1652, #13183, #142, #8100, #6492, #6799, #12978, #6595, #19431, #13283, #4915, #13081, #19537, #19742, #9887, #5020, #11482, #5223, #11688, #16355, #765, #7016, #15183, #15498, #16769, #5521, #20037, #18357, #15391, #17090, #10198, #13700, #567, #20361, #12000, #7432, #12208, #18467, #8805, #9038, #13814, #10311, #15277, #7329, #20258, #3933, #10419, #10516, #16880, #20145, #13912, #989, #5634, #5845, #13496, #12323, #19938, #16660, #12111, #4147, #16973, #18676, #15080, #7218, #10631, #2573, #2355, #2457, #18579, #660, #5416, #7109, #5735, #4039, #8922, #13589, #875, #3720, #2150, #8607, #11887, #3826, #2255, #8715, #10833, #7971, #1312, #7539, #20894, #2993, #10740, #12531, #9138, #6057, #2776, #1408, #2883, #4581, #2677, #18994, #14026, #9244, #16022, #19108, #7859, #20474, #4367, #6268, #4468, #9348, #3087, #14340, #17302, #15813, #20787, #12755, #10936, #20581, #11045, #17416, #7757, #14446, #9552, #20674, #1521, #1094, #6374, #5951, #17203, #6158, #19209, #17522, #4686, #15595, #14229, #11147, #17616, #12646, #9452, #15912, #15708, #12429, #1203, #18789, #4259, #18901, #7649, #14130, #8468, #8166, #6679, #13158 ),
 ( #16326, #1626, #14950, #18024, #4780, #6573, #3198, #115, #17832, #16426, #17929, #19608, #17725, #13052, #8078, #3305, #10077, #5085, #1915, #14547, #19404, #11551, #19709, #3490, #16534, #428, #3392, #9962, #12952, #322, #13, #6465, #19297, #5190, #1816, #6776, #4892, #3600, #8270, #11358, #221, #8376, #11660, #9858, #9765, #2018, #12853, #14743, #13256, #16230, #11247, #14847, #9667, #1715, #18130, #16132, #19507, #14637, #4996, #11461, #5494, #18333, #3906, #10172, #3799, #18648, #19916, #8685, #2224, #538, #18554, #20235, #13367, #16855, #3698, #2548, #15158, #10602, #20011, #2328, #8580, #5707, #9009, #12181, #637, #10389, #11974, #2429, #7084, #15055, #850, #2122, #19814, #13566, #16947, #18443, #16743, #739, #8781, #15254, #5394, #13675, #6985, #13473, #7191, #17064, #16634, #4010, #5297, #10490, #11769, #8895, #18234, #15476, #20124, #5603, #11863, #13786, #10283, #7303, #12084, #15367, #4117, #6881, #4662, #6036, #13885, #12508, #14104, #20451, #2749, #3062, #5931, #7407, #10712, #7735, #1384, #11123, #18972, #15569, #2856, #6241, #20330, #15888, #4442, #11014, #9322, #12402, #18874, #5816, #2658, #1063, #9215, #20557, #7510, #4346, #10813, #7830, #10908, #17277, #17491 ) ),
 .UNSPECIFIED., .F., .F., .T. ) 
 B_SPLINE_SURFACE_WITH_KNOTS ( ( 2, 2 ),
 ( 3, 2, 2, 2, 2, 2, 2, 2, 2, 2, 2, 2, 2, 2, 2, 2, 2, 2, 2, 2, 2, 2, 2, 2, 2, 2, 2, 2, 2, 2, 2, 2, 2, 2, 2, 2, 2, 2, 2, 2, 2, 2, 2, 2, 2, 2, 2, 2, 2, 2, 2, 2, 2, 2, 2, 2, 2, 2, 2, 2, 2, 2, 2, 2, 2, 2, 2, 2, 2, 2, 2, 2, 2, 2, 2, 2, 2, 2, 2, 2, 3 ),
 ( 0.000000000000000000, 1.000000000000000000 ),
 ( 0.000000000000000000, 0.01250000000000000069, 0.02500000000000000139, 0.03749999999999999861, 0.05000000000000000278, 0.06250000000000000000, 0.07499999999999999722, 0.08749999999999999445, 0.1000000000000000056, 0.1125000000000000028, 0.1250000000000000000, 0.1375000000000000111, 0.1499999999999999944, 0.1625000000000000056, 0.1749999999999999889, 0.1875000000000000000, 0.2000000000000000111, 0.2124999999999999944, 0.2250000000000000056, 0.2374999999999999889, 0.2500000000000000000, 0.2625000000000000111, 0.2750000000000000222, 0.2874999999999999778, 0.2999999999999999889, 0.3125000000000000000, 0.3250000000000000111, 0.3375000000000000222, 0.3499999999999999778, 0.3624999999999999889, 0.3750000000000000000, 0.3875000000000000111, 0.4000000000000000222, 0.4124999999999999778, 0.4249999999999999889, 0.4375000000000000000, 0.4500000000000000111, 0.4625000000000000222, 0.4749999999999999778, 0.4874999999999999889, 0.5000000000000000000, 0.5124999999999999556, 0.5250000000000000222, 0.5374999999999999778, 0.5500000000000000444, 0.5625000000000000000, 0.5749999999999999556, 0.5875000000000000222, 0.5999999999999999778, 0.6125000000000000444, 0.6250000000000000000, 0.6374999999999999556, 0.6500000000000000222, 0.6624999999999999778, 0.6750000000000000444, 0.6875000000000000000, 0.6999999999999999556, 0.7125000000000000222, 0.7249999999999999778, 0.7375000000000000444, 0.7500000000000000000, 0.7624999999999999556, 0.7750000000000000222, 0.7874999999999999778, 0.8000000000000000444, 0.8125000000000000000, 0.8249999999999999556, 0.8375000000000000222, 0.8499999999999999778, 0.8625000000000000444, 0.8750000000000000000, 0.8874999999999999556, 0.9000000000000000222, 0.9124999999999999778, 0.9250000000000000444, 0.9375000000000000000, 0.9499999999999999556, 0.9625000000000000222, 0.9749999999999999778, 0.9875000000000000444, 1.000000000000000000 ),
 .UNSPECIFIED. ) 
 GEOMETRIC_REPRESENTATION_ITEM ( )  RATIONAL_B_SPLINE_SURFACE ( (
 ( 1.000000000000000000, 0.9807852804032304306, 1.000000000000000000, 0.9807852804032304306, 1.000000000000000000, 0.9807852804032304306, 1.000000000000000000, 0.9807852804032304306, 1.000000000000000000, 0.9807852804032304306, 1.000000000000000000, 0.9807852804032304306, 1.000000000000000000, 0.9807852804032304306, 1.000000000000000000, 0.9807852804032304306, 1.000000000000000000, 0.9807852804032304306, 1.000000000000000000, 0.9807852804032304306, 1.000000000000000000, 0.9807852804032304306, 1.000000000000000000, 0.9807852804032304306, 1.000000000000000000, 0.9807852804032304306, 1.000000000000000000, 0.9807852804032304306, 1.000000000000000000, 0.9807852804032304306, 1.000000000000000000, 0.9807852804032304306, 1.000000000000000000, 0.9807852804032304306, 1.000000000000000000, 0.9807852804032304306, 1.000000000000000000, 0.9807852804032304306, 1.000000000000000000, 0.9807852804032304306, 1.000000000000000000, 0.9807852804032304306, 1.000000000000000000, 0.9807852804032304306, 1.000000000000000000, 0.9807852804032304306, 1.000000000000000000, 0.9807852804032304306, 1.000000000000000000, 0.9807852804032304306, 1.000000000000000000, 0.9807852804032304306, 1.000000000000000000, 0.9807852804032304306, 1.000000000000000000, 0.9807852804032304306, 1.000000000000000000, 0.9807852804032304306, 1.000000000000000000, 0.9807852804032304306, 1.000000000000000000, 0.9807852804032304306, 1.000000000000000000, 0.9807852804032304306, 1.000000000000000000, 0.9807852804032304306, 1.000000000000000000, 0.9807852804032304306, 1.000000000000000000, 0.9807852804032304306, 1.000000000000000000, 0.9807852804032304306, 1.000000000000000000, 0.9807852804032304306, 1.000000000000000000, 0.9807852804032304306, 1.000000000000000000, 0.9807852804032304306, 1.000000000000000000, 0.9807852804032304306, 1.000000000000000000, 0.9807852804032304306, 1.000000000000000000, 0.9807852804032304306, 1.000000000000000000, 0.9807852804032304306, 1.000000000000000000, 0.9807852804032304306, 1.000000000000000000, 0.9807852804032304306, 1.000000000000000000, 0.9807852804032304306, 1.000000000000000000, 0.9807852804032304306, 1.000000000000000000, 0.9807852804032304306, 1.000000000000000000, 0.9807852804032304306, 1.000000000000000000, 0.9807852804032304306, 1.000000000000000000, 0.9807852804032304306, 1.000000000000000000, 0.9807852804032304306, 1.000000000000000000, 0.9807852804032304306, 1.000000000000000000, 0.9807852804032304306, 1.000000000000000000, 0.9807852804032304306, 1.000000000000000000, 0.9807852804032304306, 1.000000000000000000, 0.9807852804032304306, 1.000000000000000000, 0.9807852804032304306, 1.000000000000000000, 0.9807852804032304306, 1.000000000000000000, 0.9807852804032304306, 1.000000000000000000, 0.9807852804032304306, 1.000000000000000000, 0.9807852804032304306, 1.000000000000000000, 0.9807852804032304306, 1.000000000000000000, 0.9807852804032304306, 1.000000000000000000, 0.9807852804032304306, 1.000000000000000000, 0.9807852804032304306, 1.000000000000000000, 0.9807852804032304306, 1.000000000000000000, 0.9807852804032304306, 1.000000000000000000, 0.9807852804032304306, 1.000000000000000000, 0.9807852804032304306, 1.000000000000000000, 0.9807852804032304306, 1.000000000000000000, 0.9807852804032304306, 1.000000000000000000, 0.9807852804032304306, 1.000000000000000000, 0.9807852804032304306, 1.000000000000000000, 0.9807852804032304306, 1.000000000000000000, 0.9807852804032304306, 1.000000000000000000, 0.9807852804032304306, 1.000000000000000000, 0.9807852804032304306, 1.000000000000000000, 0.9807852804032304306, 1.000000000000000000, 0.9807852804032304306, 1.000000000000000000),
 ( 1.000000000000000000, 0.9807852804032304306, 1.000000000000000000, 0.9807852804032304306, 1.000000000000000000, 0.9807852804032304306, 1.000000000000000000, 0.9807852804032304306, 1.000000000000000000, 0.9807852804032304306, 1.000000000000000000, 0.9807852804032304306, 1.000000000000000000, 0.9807852804032304306, 1.000000000000000000, 0.9807852804032304306, 1.000000000000000000, 0.9807852804032304306, 1.000000000000000000, 0.9807852804032304306, 1.000000000000000000, 0.9807852804032304306, 1.000000000000000000, 0.9807852804032304306, 1.000000000000000000, 0.9807852804032304306, 1.000000000000000000, 0.9807852804032304306, 1.000000000000000000, 0.9807852804032304306, 1.000000000000000000, 0.9807852804032304306, 1.000000000000000000, 0.9807852804032304306, 1.000000000000000000, 0.9807852804032304306, 1.000000000000000000, 0.9807852804032304306, 1.000000000000000000, 0.9807852804032304306, 1.000000000000000000, 0.9807852804032304306, 1.000000000000000000, 0.9807852804032304306, 1.000000000000000000, 0.9807852804032304306, 1.000000000000000000, 0.9807852804032304306, 1.000000000000000000, 0.9807852804032304306, 1.000000000000000000, 0.9807852804032304306, 1.000000000000000000, 0.9807852804032304306, 1.000000000000000000, 0.9807852804032304306, 1.000000000000000000, 0.9807852804032304306, 1.000000000000000000, 0.9807852804032304306, 1.000000000000000000, 0.9807852804032304306, 1.000000000000000000, 0.9807852804032304306, 1.000000000000000000, 0.9807852804032304306, 1.000000000000000000, 0.9807852804032304306, 1.000000000000000000, 0.9807852804032304306, 1.000000000000000000, 0.9807852804032304306, 1.000000000000000000, 0.9807852804032304306, 1.000000000000000000, 0.9807852804032304306, 1.000000000000000000, 0.9807852804032304306, 1.000000000000000000, 0.9807852804032304306, 1.000000000000000000, 0.9807852804032304306, 1.000000000000000000, 0.9807852804032304306, 1.000000000000000000, 0.9807852804032304306, 1.000000000000000000, 0.9807852804032304306, 1.000000000000000000, 0.9807852804032304306, 1.000000000000000000, 0.9807852804032304306, 1.000000000000000000, 0.9807852804032304306, 1.000000000000000000, 0.9807852804032304306, 1.000000000000000000, 0.9807852804032304306, 1.000000000000000000, 0.9807852804032304306, 1.000000000000000000, 0.9807852804032304306, 1.000000000000000000, 0.9807852804032304306, 1.000000000000000000, 0.9807852804032304306, 1.000000000000000000, 0.9807852804032304306, 1.000000000000000000, 0.9807852804032304306, 1.000000000000000000, 0.9807852804032304306, 1.000000000000000000, 0.9807852804032304306, 1.000000000000000000, 0.9807852804032304306, 1.000000000000000000, 0.9807852804032304306, 1.000000000000000000, 0.9807852804032304306, 1.000000000000000000, 0.9807852804032304306, 1.000000000000000000, 0.9807852804032304306, 1.000000000000000000, 0.9807852804032304306, 1.000000000000000000, 0.9807852804032304306, 1.000000000000000000, 0.9807852804032304306, 1.000000000000000000, 0.9807852804032304306, 1.000000000000000000, 0.9807852804032304306, 1.000000000000000000, 0.9807852804032304306, 1.000000000000000000, 0.9807852804032304306, 1.000000000000000000, 0.9807852804032304306, 1.000000000000000000, 0.9807852804032304306, 1.000000000000000000, 0.9807852804032304306, 1.000000000000000000, 0.9807852804032304306, 1.000000000000000000, 0.9807852804032304306, 1.000000000000000000, 0.9807852804032304306, 1.000000000000000000, 0.9807852804032304306, 1.000000000000000000, 0.9807852804032304306, 1.000000000000000000, 0.9807852804032304306, 1.000000000000000000, 0.9807852804032304306, 1.000000000000000000, 0.9807852804032304306, 1.000000000000000000) ) ) 
 REPRESENTATION_ITEM ( '' )  SURFACE ( )  );
#11698 = ORIENTED_EDGE ( 'NONE', *, *, #15336, .F. ) ;
#11699 = EDGE_CURVE ( 'NONE', #15235, #18900, #6973, .T. ) ;
#11700 = DIRECTION ( 'NONE',  ( -1.000000000000000000, 0.000000000000000000, 0.000000000000000000 ) ) ;
#11701 = SURFACE_SIDE_STYLE ('',( #13407 ) ) ;
#11702 = EDGE_CURVE ( 'NONE', #7786, #19208, #562, .T. ) ;
#11703 = ADVANCED_FACE ( 'NONE', ( #3346 ), #9807, .F. ) ;
#11704 = CIRCLE ( 'NONE', #187, 27.60000000002759535 ) ;
#11705 = CARTESIAN_POINT ( 'NONE',  ( 30.00000000000000000, -170.8299878242309546, 15.48896927112552824 ) ) ;
#11706 =( REPRESENTATION_RELATIONSHIP ('NONE','NONE', #13739, #8160 ) REPRESENTATION_RELATIONSHIP_WITH_TRANSFORMATION ( #7051 )SHAPE_REPRESENTATION_RELATIONSHIP( ) );
#11707 = CARTESIAN_POINT ( 'NONE',  ( 9.474249097082498849, -6.330490858644140850, 7.951203500647429756 ) ) ;
#11708 = VERTEX_POINT ( 'NONE', #11406 ) ;
#11709 = VECTOR ( 'NONE', #5728, 1000.000000000000000 ) ;
#11710 = ADVANCED_FACE ( 'NONE', ( #1764 ), #8217, .T. ) ;
#11711 = DIRECTION ( 'NONE',  ( 0.000000000000000000, 0.000000000000000000, 1.000000000000000000 ) ) ;
#11712 = ORIENTED_EDGE ( 'NONE', *, *, #10981, .F. ) ;
#11713 = CARTESIAN_POINT ( 'NONE',  ( 6.358192987158592047, -4.248408730893246776, -27.01760624981969627 ) ) ;
#11714 = ORIENTED_EDGE ( 'NONE', *, *, #2472, .T. ) ;
#11715 = CARTESIAN_POINT ( 'NONE',  ( -12.72792205982779912, 12.72792206288790950, 10.34917500018031333 ) ) ;
#11716 = CARTESIAN_POINT ( 'NONE',  ( 19.99999999999999645, 61.72688495901586947, 19.84591825364119089 ) ) ;
#11717 = CARTESIAN_POINT ( 'NONE',  ( 50.00000000000000000, -170.8299878242309546, 15.48896927112552824 ) ) ;
#11718 = VERTEX_POINT ( 'NONE', #3443 ) ;
#11719 = AXIS2_PLACEMENT_3D ( 'NONE', #17534, #7868, #20797 ) ;
#11720 = CARTESIAN_POINT ( 'NONE',  ( 2.500000000000000000, 1.768423874527823791, 1.020999999999998353 ) ) ;
#11721 = ORIENTED_EDGE ( 'NONE', *, *, #8285, .F. ) ;
#11722 = CARTESIAN_POINT ( 'NONE',  ( 0.000000000000000000, -48.70996102988709708, 42.79495875147758710 ) ) ;
#11723 = AXIS2_PLACEMENT_3D ( 'NONE', #5574, #18417, #8655 ) ;
#11724 = VECTOR ( 'NONE', #17352, 1000.000000000000000 ) ;
#11725 = ORIENTED_EDGE ( 'NONE', *, *, #17772, .F. ) ;
#11726 = CARTESIAN_POINT ( 'NONE',  ( 9.999999999999998224, -71.89099403602352822, -3.960426305689549675 ) ) ;
#11727 = VECTOR ( 'NONE', #8723, 1000.000000000000000 ) ;
#11728 = CARTESIAN_POINT ( 'NONE',  ( 85.00002539999999840, 0.000000000000000000, 0.000000000000000000 ) ) ;
#11729 = APPLICATION_PROTOCOL_DEFINITION ( 'draft international standard', 'automotive_design', 1998, #18324 ) ;
#11730 = CARTESIAN_POINT ( 'NONE',  ( -13.67243654642775574, 5.663308650141533285, 11.61685441884154812 ) ) ;
#11731 = ORIENTED_EDGE ( 'NONE', *, *, #19332, .T. ) ;
#11732 = AXIS2_PLACEMENT_3D ( 'NONE', #10160, #16414, #4982 ) ;
#11733 = CIRCLE ( 'NONE', #17160, 72.00000000007199219 ) ;
#11734 = CARTESIAN_POINT ( 'NONE',  ( 19.99999999999999645, -23.08379033237394395, 61.02926039941428371 ) ) ;
#11735 = DIRECTION ( 'NONE',  ( -1.000000000000000000, 0.000000000000000000, 0.000000000000000000 ) ) ;
#11736 = AXIS2_PLACEMENT_3D ( 'NONE', #3274, #19678, #3465 ) ;
#11737 = CARTESIAN_POINT ( 'NONE',  ( -2.943691925285395694, 14.79893867793683349, -20.80357316848093063 ) ) ;
#11738 = COLOUR_RGB ( '', 0.40784314, 0.44705882, 0.49803922) ;
#11739 = CARTESIAN_POINT ( 'NONE',  ( 19.99999999999999645, -51.81019761368295207, -38.98425606966110735 ) ) ;
#11740 = VERTEX_POINT ( 'NONE', #19963 ) ;
#11741 = EDGE_CURVE ( 'NONE', #17356, #988, #13939, .T. ) ;
#11742 = CYLINDRICAL_SURFACE ( 'NONE', #5627, 2.649999999999992806 ) ;
#11743 = CARTESIAN_POINT ( 'NONE',  ( -1.491842754445841690, 7.500000000179340987, 16.57301875018031012 ) ) ;
#11744 = VERTEX_POINT ( 'NONE', #13619 ) ;
#11745 = CARTESIAN_POINT ( 'NONE',  ( 0.000000000000000000, 70.29359119158485214, 15.58239511117312226 ) ) ;
#11746 = VERTEX_POINT ( 'NONE', #12027 ) ;
#11747 = CARTESIAN_POINT ( 'NONE',  ( 30.00000000000000000, -164.9999999999999716, 50.00000000000001421 ) ) ;
#11748 = CARTESIAN_POINT ( 'NONE',  ( 15.25966317163202568, 10.19618095047498230, 11.09535625018031091 ) ) ;
#11749 = CIRCLE ( 'NONE', #1617, 65.24900000006525147 ) ;
#11750 = VERTEX_POINT ( 'NONE', #3746 ) ;
#11751 = ORIENTED_EDGE ( 'NONE', *, *, #6195, .T. ) ;
#11752 = DIRECTION ( 'NONE',  ( -1.000000000000000000, 0.000000000000000000, 0.000000000000000000 ) ) ;
#11753 = AXIS2_PLACEMENT_3D ( 'NONE', #1465, #13316, #995 ) ;
#11754 = VECTOR ( 'NONE', #8117, 1000.000000000000000 ) ;
#11755 = DIRECTION ( 'NONE',  ( -1.000000000000000000, -0.000000000000000000, -0.000000000000000000 ) ) ;
#11756 = CYLINDRICAL_SURFACE ( 'NONE', #8866, 7.500000000000000000 ) ;
#11757 =( NAMED_UNIT ( * ) PLANE_ANGLE_UNIT ( ) SI_UNIT ( $, .RADIAN. ) );
#11758 = CARTESIAN_POINT ( 'NONE',  ( 3.580422610670021211, -18.00000000043041481, 15.94526875018031298 ) ) ;
#11759 = DIRECTION ( 'NONE',  ( -1.000000000000000000, 0.000000000000000000, 0.000000000000000000 ) ) ;
#11760 = CARTESIAN_POINT ( 'NONE',  ( -5.303300859536636658, -5.303300858261589035, -8.676924999819688011 ) ) ;
#11761 = VECTOR ( 'NONE', #3043, 1000.000000000000000 ) ;
#11762 = CARTESIAN_POINT ( 'NONE',  ( -7.902369978624323110, -7.902369976724391343, -15.37073475028680569 ) ) ;
#11763 = DIRECTION ( 'NONE',  ( 0.000000000000000000, 0.000000000000000000, 1.000000000000000000 ) ) ;
#11764 = DIRECTION ( 'NONE',  ( 0.000000000000000000, -1.000000000000000000, 0.000000000000000000 ) ) ;
#11765 = AXIS2_PLACEMENT_3D ( 'NONE', #18641, #15360, #20323 ) ;
#11766 = ORIENTED_EDGE ( 'NONE', *, *, #2345, .T. ) ;
#11767 = ADVANCED_FACE ( 'NONE', ( #15207 ), #12235, .F. ) ;
#11768 = CARTESIAN_POINT ( 'NONE',  ( 0.000000000000000000, 20.60847369612982405, 61.90898814327722732 ) ) ;
#11769 = CARTESIAN_POINT ( 'NONE',  ( -16.62983158437510056, 6.888301784570729502, -9.089887499819687022 ) ) ;
#11770 = LINE ( 'NONE', #7085, #17080 ) ;
#11771 = VERTEX_POINT ( 'NONE', #18387 ) ;
#11772 = CARTESIAN_POINT ( 'NONE',  ( 19.99999999999999645, -20.60847369613026103, 61.90898814327709943 ) ) ;
#11773 = VERTEX_POINT ( 'NONE', #10545 ) ;
#11774 = FACE_BOUND ( 'NONE', #19439, .T. ) ;
#11775 = DIRECTION ( 'NONE',  ( 0.000000000000000000, 0.000000000000000000, -1.000000000000000000 ) ) ;
#11776 = VERTEX_POINT ( 'NONE', #10228 ) ;
#11777 = ORIENTED_EDGE ( 'NONE', *, *, #17155, .F. ) ;
#11778 = DIRECTION ( 'NONE',  ( -1.000000000000000000, 0.000000000000000000, 0.000000000000000000 ) ) ;
#11779 = ADVANCED_FACE ( 'NONE', ( #20396, #20068 ), #20281, .F. ) ;
#11780 = DIRECTION ( 'NONE',  ( -1.000000000000000000, 0.000000000000000000, 0.000000000000000000 ) ) ;
#11781 = DIRECTION ( 'NONE',  ( -1.000000000000000000, 0.000000000000000000, 0.000000000000000000 ) ) ;
#11782 = EDGE_CURVE ( 'NONE', #14994, #17908, #2604, .T. ) ;
#11783 = CARTESIAN_POINT ( 'NONE',  ( 1.491842756249028845, 7.499999999820661678, 17.16208125018031438 ) ) ;
#11784 = DIRECTION ( 'NONE',  ( 0.000000000000000000, 0.000000000000000000, 1.000000000000000000 ) ) ;
#11785 = CARTESIAN_POINT ( 'NONE',  ( 9.999999999999998224, -71.76067541710847308, -5.865617076725375689 ) ) ;
#11786 = CARTESIAN_POINT ( 'NONE',  ( 19.99999999999999645, 5.762283366691162811, 64.99406197038673838 ) ) ;
#11787 = CARTESIAN_POINT ( 'NONE',  ( -4.000000000000000000, -1.933795701539610556, -0.2488376576622980119 ) ) ;
#11788 = ORIENTED_EDGE ( 'NONE', *, *, #9485, .T. ) ;
#11789 = DIRECTION ( 'NONE',  ( -0.000000000000000000, -0.000000000000000000, -1.000000000000000000 ) ) ;
#11790 = ORIENTED_EDGE ( 'NONE', *, *, #18207, .T. ) ;
#11791 = CARTESIAN_POINT ( 'NONE',  ( 18.00000000000000000, -2.163824016901520184E-09, 21.40395000018031624 ) ) ;
#11792 = CARTESIAN_POINT ( 'NONE',  ( -7.539743116613911944, -20.19060691129837437, 71.13878616268864619 ) ) ;
#11793 = EDGE_LOOP ( 'NONE', ( #6821, #19636 ) ) ;
#11794 = DIRECTION ( 'NONE',  ( 1.000000000000000000, 0.000000000000000000, 0.000000000000000000 ) ) ;
#11795 = EDGE_LOOP ( 'NONE', ( #18501, #16067 ) ) ;
#11796 = LINE ( 'NONE', #5229, #12890 ) ;
#11797 = CARTESIAN_POINT ( 'NONE',  ( -31.74999999999995737, 0.000000000000000000, 4.250000000000000000 ) ) ;
#11798 = VERTEX_POINT ( 'NONE', #3963 ) ;
#11799 = EDGE_CURVE ( 'NONE', #9794, #8219, #3856, .T. ) ;
#11800 = ADVANCED_FACE ( 'NONE', ( #5760 ), #1014, .F. ) ;
#11801 = DIRECTION ( 'NONE',  ( 1.000000000000000000, -0.000000000000000000, -0.000000000000000000 ) ) ;
#11802 = CARTESIAN_POINT ( 'NONE',  ( -12.72792205982779556, 12.72792206288790773, -10.40542499981968838 ) ) ;
#11803 = SURFACE_STYLE_USAGE ( .BOTH. , #11701 ) ;
#11804 = EDGE_CURVE ( 'NONE', #3682, #17307, #11068, .T. ) ;
#11805 = CARTESIAN_POINT ( 'NONE',  ( 9.999999999999998224, 36.59093685910711002, -62.00889726307995176 ) ) ;
#11806 = ADVANCED_FACE ( 'NONE', ( #7042 ), #7135, .F. ) ;
#11807 = CARTESIAN_POINT ( 'NONE',  ( 11.17563879731705789, -1.343450868547281933E-09, 16.49260975064743562 ) ) ;
#11808 = VERTEX_POINT ( 'NONE', #11816 ) ;
#11809 = CARTESIAN_POINT ( 'NONE',  ( 0.2500000000000002220, 0.000000000000000000, 4.250000000000000000 ) ) ;
#11810 = DIRECTION ( 'NONE',  ( -0.000000000000000000, -0.000000000000000000, -1.000000000000000000 ) ) ;
#11811 = ORIENTED_EDGE ( 'NONE', *, *, #15288, .F. ) ;
#11812 = CARTESIAN_POINT ( 'NONE',  ( -19.56401537842534921, -8.921674172384493673, -77.87798366923529159 ) ) ;
#11813 = ORIENTED_EDGE ( 'NONE', *, *, #12572, .T. ) ;
#11814 = CARTESIAN_POINT ( 'NONE',  ( 15.25966317163202746, 10.19618095047498407, 3.574956250180311379 ) ) ;
#11815 = DIRECTION ( 'NONE',  ( 0.000000000000000000, 0.000000000000000000, -1.000000000000000000 ) ) ;
#11816 = CARTESIAN_POINT ( 'NONE',  ( 19.99999999999999645, 45.48683723007275148, -46.78012013466171481 ) ) ;
#11817 = EDGE_CURVE ( 'NONE', #2521, #8637, #6645, .T. ) ;
#11818 = EDGE_CURVE ( 'NONE', #16910, #8415, #10661, .T. ) ;
#11819 = EDGE_LOOP ( 'NONE', ( #5552, #4308 ) ) ;
#11820 = DIRECTION ( 'NONE',  ( 1.000000000000000000, 0.000000000000000000, -0.000000000000000000 ) ) ;
#11821 = EDGE_LOOP ( 'NONE', ( #667, #15133, #15039, #17703 ) ) ;
#11822 = CARTESIAN_POINT ( 'NONE',  ( 30.00000000000000000, -159.9999999999999716, -53.99496054166690584 ) ) ;
#11823 = EDGE_CURVE ( 'NONE', #10704, #12901, #5550, .T. ) ;
#11824 = APPLICATION_CONTEXT ( 'automotive_design' ) ;
#11825 = ORIENTED_EDGE ( 'NONE', *, *, #2561, .F. ) ;
#11826 = LINE ( 'NONE', #12142, #9050 ) ;
#11827 = ADVANCED_FACE ( 'NONE', ( #18497 ), #8740, .T. ) ;
#11828 = CYLINDRICAL_SURFACE ( 'NONE', #17711, 72.00000000007199219 ) ;
#11829 = CARTESIAN_POINT ( 'NONE',  ( -5.663308650141539502, -13.67243654642775574, 18.68560441884154599 ) ) ;
#11830 = ORIENTED_EDGE ( 'NONE', *, *, #6233, .T. ) ;
#11831 = CARTESIAN_POINT ( 'NONE',  ( 0.000000000000000000, -27.62776854598816101, -58.65812137499030854 ) ) ;
#11832 = ORIENTED_EDGE ( 'NONE', *, *, #19286, .T. ) ;
#11833 = CARTESIAN_POINT ( 'NONE',  ( 17.00000000000000000, 0.000000000000000000, 2.055000000000000160 ) ) ;
#11834 = VECTOR ( 'NONE', #5899, 1000.000000000000000 ) ;
#11835 = CARTESIAN_POINT ( 'NONE',  ( -17.99999999956958163, 3.580422614997673669, 16.98598125018030913 ) ) ;
#11836 = CARTESIAN_POINT ( 'NONE',  ( 0.000000000000000000, -71.76067541710854414, 5.865617076724380041 ) ) ;
#11837 = EDGE_CURVE ( 'NONE', #9969, #15420, #15419, .T. ) ;
#11838 = EDGE_LOOP ( 'NONE', ( #9429, #13125, #2454, #14094 ) ) ;
#11839 = CARTESIAN_POINT ( 'NONE',  ( 38.20577202892028623, -121.1578191933347739, 85.85343169282300835 ) ) ;
#11840 = FACE_BOUND ( 'NONE', #14194, .T. ) ;
#11841 = ORIENTED_EDGE ( 'NONE', *, *, #10940, .F. ) ;
#11842 = CARTESIAN_POINT ( 'NONE',  ( 0.000000000000000000, 11.98658579560678206, -64.13855129306456604 ) ) ;
#11843 = ORIENTED_EDGE ( 'NONE', *, *, #4720, .F. ) ;
#11844 = CARTESIAN_POINT ( 'NONE',  ( 50.00000000000000000, -3.649167310370820871, 90.00000000000000000 ) ) ;
#11845 = CARTESIAN_POINT ( 'NONE',  ( 17.99999999956957808, -3.580422614997675446, 2.848481250180310287 ) ) ;
#11846 = ORIENTED_EDGE ( 'NONE', *, *, #14919, .F. ) ;
#11847 = ORIENTED_EDGE ( 'NONE', *, *, #4539, .F. ) ;
#11848 = DIRECTION ( 'NONE',  ( -0.000000000000000000, 1.000000000000000000, 0.000000000000000000 ) ) ;
#11849 = VECTOR ( 'NONE', #7008, 1000.000000000000000 ) ;
#11850 = DIRECTION ( 'NONE',  ( -1.000000000000000000, 0.000000000000000000, 0.000000000000000000 ) ) ;
#11851 = DIRECTION ( 'NONE',  ( -1.000000000000000000, 0.000000000000000000, 0.000000000000000000 ) ) ;
#11852 = DIRECTION ( 'NONE',  ( 0.000000000000000000, 0.000000000000000000, 1.000000000000000000 ) ) ;
#11853 = EDGE_CURVE ( 'NONE', #20507, #14958, #12135, .T. ) ;
#11854 = LINE ( 'NONE', #15243, #4232 ) ;
#11855 = CARTESIAN_POINT ( 'NONE',  ( -4.248408729364580694, 6.358192988180020322, -6.026143749819683038 ) ) ;
#11856 = CIRCLE ( 'NONE', #15921, 65.24900000006525147 ) ;
#11857 = CARTESIAN_POINT ( 'NONE',  ( 7.902369976724389566, -7.902369978624323110, -17.72698475028679965 ) ) ;
#11858 = CARTESIAN_POINT ( 'NONE',  ( 21.50000000000000000, 2.632990618166809235E-15, -68.00000000000000000 ) ) ;
#11859 = DIRECTION ( 'NONE',  ( -1.000000000000000000, -0.000000000000000000, 0.000000000000000000 ) ) ;
#11860 = ORIENTED_EDGE ( 'NONE', *, *, #8584, .F. ) ;
#11861 = CARTESIAN_POINT ( 'NONE',  ( 0.000000000000000000, 0.000000000000000000, -43.00000000000000000 ) ) ;
#11862 = AXIS2_PLACEMENT_3D ( 'NONE', #13199, #14789, #269 ) ;
#11863 = CARTESIAN_POINT ( 'NONE',  ( -12.72792206288791128, -12.72792205982779912, -10.85707499981969093 ) ) ;
#11864 = DIRECTION ( 'NONE',  ( 0.000000000000000000, 0.000000000000000000, 1.000000000000000000 ) ) ;
#11865 = ORIENTED_EDGE ( 'NONE', *, *, #4791, .F. ) ;
#11866 = CARTESIAN_POINT ( 'NONE',  ( -30.00000000000000000, -170.8299878242309546, -15.48896927112552824 ) ) ;
#11867 = VERTEX_POINT ( 'NONE', #907 ) ;
#11868 = DIRECTION ( 'NONE',  ( 1.000000000000000000, 0.000000000000000000, 0.000000000000000000 ) ) ;
#11869 = FACE_BOUND ( 'NONE', #15872, .T. ) ;
#11870 = ORIENTED_EDGE ( 'NONE', *, *, #1077, .T. ) ;
#11871 = AXIS2_PLACEMENT_3D ( 'NONE', #8474, #14748, #12957 ) ;
#11872 = EDGE_LOOP ( 'NONE', ( #9549, #12370, #14586, #13168 ) ) ;
#11873 = CARTESIAN_POINT ( 'NONE',  ( 0.000000000000000000, 0.000000000000000000, 46.00000000000000711 ) ) ;
#11874 = FILL_AREA_STYLE_COLOUR ( '', #13442 ) ;
#11875 = DIRECTION ( 'NONE',  ( 0.000000000000000000, -1.000000000000000000, 0.000000000000000000 ) ) ;
#11876 = EDGE_CURVE ( 'NONE', #3628, #798, #13774, .T. ) ;
#11877 = DIRECTION ( 'NONE',  ( -1.000000000000000000, 0.000000000000000000, 0.000000000000000000 ) ) ;
#11878 = AXIS2_PLACEMENT_3D ( 'NONE', #3016, #14569, #8193 ) ;
#11879 = CARTESIAN_POINT ( 'NONE',  ( -5.303300858261583706, 5.303300859536630441, -3.160574999819688369 ) ) ;
#11880 = CARTESIAN_POINT ( 'NONE',  ( 50.00000000000000000, -3.649167310370820871, 90.00000000000000000 ) ) ;
#11881 = FACE_OUTER_BOUND ( 'NONE', #1015, .T. ) ;
#11882 = LINE ( 'NONE', #559, #5767 ) ;
#11883 = CARTESIAN_POINT ( 'NONE',  ( 0.000000000000000000, -68.15657073222450890, 23.20952102120257976 ) ) ;
#11884 = ORIENTED_EDGE ( 'NONE', *, *, #13216, .F. ) ;
#11885 = DIRECTION ( 'NONE',  ( 0.6156453966108041964, 0.000000000000000000, -0.7880233154113687188 ) ) ;
#11886 = ORIENTED_EDGE ( 'NONE', *, *, #2948, .T. ) ;
#11887 = CARTESIAN_POINT ( 'NONE',  ( 3.580422610670020322, -18.00000000043041126, -4.809331249819685183 ) ) ;
#11888 = DIRECTION ( 'NONE',  ( -1.000000000000000000, 0.000000000000000000, 0.000000000000000000 ) ) ;
#11889 = CIRCLE ( 'NONE', #6145, 65.24900000006525147 ) ;
#11890 = ORIENTED_EDGE ( 'NONE', *, *, #14818, .F. ) ;
#11891 = CARTESIAN_POINT ( 'NONE',  ( 5.000000000000000888, 0.000000000000000000, 0.000000000000000000 ) ) ;
#11892 = ORIENTED_EDGE ( 'NONE', *, *, #13222, .F. ) ;
#11893 = CARTESIAN_POINT ( 'NONE',  ( 30.00000000000000711, 29.99999999999998579, -120.0000000000000142 ) ) ;
#11894 = CYLINDRICAL_SURFACE ( 'NONE', #6978, 20.00000000000000355 ) ;
#11895 = EDGE_LOOP ( 'NONE', ( #791, #20653, #463, #1504 ) ) ;
#11896 = AXIS2_PLACEMENT_3D ( 'NONE', #3968, #8840, #7044 ) ;
#11897 = CARTESIAN_POINT ( 'NONE',  ( 6.358192988180014993, 4.248408729364578917, -9.934793749819693431 ) ) ;
#11898 = CARTESIAN_POINT ( 'NONE',  ( 3.580422614997667896, 17.99999999956958163, -8.932768749819693710 ) ) ;
#11899 = CARTESIAN_POINT ( 'NONE',  ( 30.00000000000000000, -97.49621075554985339, 111.6458212409894486 ) ) ;
#11900 = DIRECTION ( 'NONE',  ( -1.000000000000000000, 0.000000000000000000, 0.000000000000000000 ) ) ;
#11901 = MECHANICAL_DESIGN_GEOMETRIC_PRESENTATION_REPRESENTATION (  '', ( #9209 ), #748 ) ;
#11902 = CARTESIAN_POINT ( 'NONE',  ( -10.32494394706616703, 4.276731815070943910, 12.36917225064743242 ) ) ;
#11903 = ORIENTED_EDGE ( 'NONE', *, *, #17248, .T. ) ;
#11904 = DIRECTION ( 'NONE',  ( -1.000000000000000000, 0.000000000000000000, 0.000000000000000000 ) ) ;
#11905 = CARTESIAN_POINT ( 'NONE',  ( 20.00000000000000355, 0.000000000000000000, 0.000000000000000000 ) ) ;
#11906 = ORIENTED_EDGE ( 'NONE', *, *, #4929, .F. ) ;
#11907 = CARTESIAN_POINT ( 'NONE',  ( -18.69829135368511430, -10.63264222386860958, -76.60301815488040234 ) ) ;
#11908 = EDGE_CURVE ( 'NONE', #13280, #3180, #18926, .T. ) ;
#11909 = VECTOR ( 'NONE', #14417, 1000.000000000000000 ) ;
#11910 = ORIENTED_EDGE ( 'NONE', *, *, #824, .T. ) ;
#11911 = ADVANCED_FACE ( 'NONE', ( #1338 ), #1546, .F. ) ;
#11912 = CARTESIAN_POINT ( 'NONE',  ( 15.25966316918061416, -10.19618095414378622, 14.76714375018031333 ) ) ;
#11913 = CIRCLE ( 'NONE', #2789, 4.000000000000000888 ) ;
#11914 = CARTESIAN_POINT ( 'NONE',  ( 19.99999999999999645, 0.000000000000000000, 0.000000000000000000 ) ) ;
#11915 = CARTESIAN_POINT ( 'NONE',  ( 0.000000000000000000, 0.000000000000000000, -25.03750572909317285 ) ) ;
#11916 = ORIENTED_EDGE ( 'NONE', *, *, #9510, .T. ) ;
#11917 = ORIENTED_EDGE ( 'NONE', *, *, #17291, .F. ) ;
#11918 = CARTESIAN_POINT ( 'NONE',  ( 19.99999999999999645, -60.40676135667420965, -23.56039007469101421 ) ) ;
#11919 = EDGE_CURVE ( 'NONE', #16951, #742, #6190, .T. ) ;
#11920 = VERTEX_POINT ( 'NONE', #9166 ) ;
#11921 = DIRECTION ( 'NONE',  ( 0.000000000000000000, 0.9976687691905394839, -0.06824241336466758956 ) ) ;
#11922 = ORIENTED_EDGE ( 'NONE', *, *, #20111, .T. ) ;
#11923 = DIRECTION ( 'NONE',  ( 0.000000000000000000, -0.8169698930104354329, -0.5766803221148765202 ) ) ;
#11924 = AXIS2_PLACEMENT_3D ( 'NONE', #382, #16588, #11618 ) ;
#11925 = CIRCLE ( 'NONE', #14648, 65.24900000006526568 ) ;
#11926 = CARTESIAN_POINT ( 'NONE',  ( 19.99999999999999645, -39.37110852956777762, -51.51683813304910586 ) ) ;
#11927 = CIRCLE ( 'NONE', #9233, 11.50000000000000000 ) ;
#11928 = CARTESIAN_POINT ( 'NONE',  ( 14.79893867758297610, -1.779016607511492805E-09, 15.74029191884154599 ) ) ;
#11929 = ADVANCED_FACE ( 'NONE', ( #16053 ), #20814, .T. ) ;
#11930 = EDGE_LOOP ( 'NONE', ( #18420, #2779, #16134, #9475 ) ) ;
#11931 = DIRECTION ( 'NONE',  ( -1.000000000000000000, 0.000000000000000000, 0.000000000000000000 ) ) ;
#11932 = ORIENTED_EDGE ( 'NONE', *, *, #17740, .T. ) ;
#11933 = AXIS2_PLACEMENT_3D ( 'NONE', #1138, #7474, #13957 ) ;
#11934 =( BOUNDED_CURVE ( )  B_SPLINE_CURVE ( 2, ( #15755, #12696, #7596, #17570, #9295, #14073, #6007, #20525, #12478, #17461, #10986, #15959, #1256, #2935, #1460, #5781, #12257 ),
 .UNSPECIFIED., .F., .T. ) 
 B_SPLINE_CURVE_WITH_KNOTS ( ( 3, 2, 2, 2, 2, 2, 2, 2, 3 ),
 ( 0.8000000000038511860, 0.8125000000038511416, 0.8250000000038510972, 0.8375000000038511638, 0.8500000000038511194, 0.8625000000038511860, 0.8750000000038511416, 0.8875000000038510972, 0.9000000000038511638 ),
 .UNSPECIFIED. ) 
 CURVE ( )  GEOMETRIC_REPRESENTATION_ITEM ( )  RATIONAL_B_SPLINE_CURVE ( ( 0.9999999999940800688, 0.9807852804091503618, 1.000000000000000000, 0.9807852804032304306, 1.000000000000000000, 0.9807852804032304306, 1.000000000000000000, 0.9807852804032304306, 1.000000000000000000, 0.9807852804032304306, 1.000000000000000000, 0.9807852804032304306, 1.000000000000000000, 0.9807852804032304306, 1.000000000000000000, 0.9807852803973104994, 1.000000000005919931 ) ) 
 REPRESENTATION_ITEM ( '' )  );
#11935 = CARTESIAN_POINT ( 'NONE',  ( 0.000000000000000000, 0.000000000000000000, 90.00000000000000000 ) ) ;
#11936 = EDGE_CURVE ( 'NONE', #5449, #2438, #7582, .T. ) ;
#11937 = CARTESIAN_POINT ( 'NONE',  ( 17.99999999999999645, -2.163824016901520184E-09, 21.40395000018031268 ) ) ;
#11938 = EDGE_CURVE ( 'NONE', #16003, #17243, #17070, .T. ) ;
#11939 = DIRECTION ( 'NONE',  ( 1.000000000000000000, 0.000000000000000000, 0.000000000000000000 ) ) ;
#11940 = AXIS2_PLACEMENT_3D ( 'NONE', #3454, #13217, #4952 ) ;
#11941 = VECTOR ( 'NONE', #17306, 1000.000000000000000 ) ;
#11942 = ORIENTED_EDGE ( 'NONE', *, *, #14282, .T. ) ;
#11943 = EDGE_CURVE ( 'NONE', #7282, #14001, #18772, .T. ) ;
#11944 = DIRECTION ( 'NONE',  ( 0.000000000000000000, 0.000000000000000000, 1.000000000000000000 ) ) ;
#11945 = DIRECTION ( 'NONE',  ( 1.000000000000000000, 0.000000000000000000, 0.000000000000000000 ) ) ;
#11946 = ORIENTED_EDGE ( 'NONE', *, *, #10869, .T. ) ;
#11947 = CYLINDRICAL_SURFACE ( 'NONE', #19378, 27.60000000002759890 ) ;
#11948 = ORIENTED_EDGE ( 'NONE', *, *, #150, .T. ) ;
#11949 = DIRECTION ( 'NONE',  ( -1.000000000000000000, -0.000000000000000000, -0.000000000000000000 ) ) ;
#11950 = CARTESIAN_POINT ( 'NONE',  ( -6.888301780572500199, 16.62983158603121936, 9.033637500180310198 ) ) ;
#11951 = ORIENTED_EDGE ( 'NONE', *, *, #14911, .F. ) ;
#11952 = AXIS2_PLACEMENT_3D ( 'NONE', #5824, #14110, #1187 ) ;
#11953 = ORIENTED_EDGE ( 'NONE', *, *, #11283, .T. ) ;
#11954 = DIRECTION ( 'NONE',  ( -1.000000000000000000, 0.000000000000000000, 0.000000000000000000 ) ) ;
#11955 = CIRCLE ( 'NONE', #6210, 5.000000000000004441 ) ;
#11956 = CARTESIAN_POINT ( 'NONE',  ( 7.500000000000001776, -9.015933403756337545E-10, 22.35625000018031017 ) ) ;
#11957 = DIRECTION ( 'NONE',  ( -1.000000000000000000, 0.000000000000000000, -0.000000000000000000 ) ) ;
#11958 =( NAMED_UNIT ( * ) SI_UNIT ( $, .STERADIAN. ) SOLID_ANGLE_UNIT ( ) );
#11959 = CARTESIAN_POINT ( 'NONE',  ( 6.249999999999902300, -10.82531754730554496, 169.0000000000000000 ) ) ;
#11960 = AXIS2_PLACEMENT_3D ( 'NONE', #1349, #5120, #8508 ) ;
#11961 = AXIS2_PLACEMENT_3D ( 'NONE', #14746, #6576, #13055 ) ;
#11962 = EDGE_CURVE ( 'NONE', #16164, #10495, #5537, .T. ) ;
#11963 = PRODUCT_DEFINITION_CONTEXT ( 'detailed design', #189, 'design' ) ;
#11964 = DIRECTION ( 'NONE',  ( -1.000000000000000000, -0.000000000000000000, -0.000000000000000000 ) ) ;
#11965 = CARTESIAN_POINT ( 'NONE',  ( -7.500000000000007994, 9.015942588607339023E-10, 1.926200000180313454 ) ) ;
#11966 = FACE_OUTER_BOUND ( 'NONE', #8511, .T. ) ;
#11967 = CARTESIAN_POINT ( 'NONE',  ( 11.17563879758427525, 2.222972768810836719, -19.19964100028681031 ) ) ;
#11968 = EDGE_CURVE ( 'NONE', #20902, #4551, #12339, .T. ) ;
#11969 = CIRCLE ( 'NONE', #5182, 20.00000000000000355 ) ;
#11970 = DIRECTION ( 'NONE',  ( 0.000000000000000000, 0.000000000000000000, 1.000000000000000000 ) ) ;
#11971 = VECTOR ( 'NONE', #11515, 1000.000000000000000 ) ;
#11972 = VERTEX_POINT ( 'NONE', #12353 ) ;
#11973 = DIRECTION ( 'NONE',  ( 0.000000000000000000, 0.000000000000000000, 1.000000000000000000 ) ) ;
#11974 = CARTESIAN_POINT ( 'NONE',  ( -6.888301784570738384, -16.62983158437509346, -2.021137499819688266 ) ) ;
#11975 = DIRECTION ( 'NONE',  ( -1.000000000000000000, 0.000000000000000000, 0.000000000000000000 ) ) ;
#11976 = VECTOR ( 'NONE', #4700, 1000.000000000000000 ) ;
#11977 = ORIENTED_EDGE ( 'NONE', *, *, #1611, .F. ) ;
#11978 = DIRECTION ( 'NONE',  ( 0.000000000000000000, -0.9790840876823249106, 0.2034560130526240906 ) ) ;
#11979 = EDGE_LOOP ( 'NONE', ( #20214, #8479, #5124, #2760 ) ) ;
#11980 = AXIS2_PLACEMENT_3D ( 'NONE', #8196, #11483, #8101 ) ;
#11981 = CARTESIAN_POINT ( 'NONE',  ( 19.99999999999999645, -58.44960523466222213, -28.06621538408651872 ) ) ;
#11982 = DIRECTION ( 'NONE',  ( -0.000000000000000000, 0.000000000000000000, -1.000000000000000000 ) ) ;
#11983 = ORIENTED_EDGE ( 'NONE', *, *, #14052, .F. ) ;
#11984 = ORIENTED_EDGE ( 'NONE', *, *, #9696, .T. ) ;
#11985 = DIRECTION ( 'NONE',  ( -1.000000000000000000, -0.000000000000000000, -0.000000000000000000 ) ) ;
#11986 = CIRCLE ( 'NONE', #17059, 2.649999999999999467 ) ;
#11987 = SURFACE_SIDE_STYLE ('',( #7097 ) ) ;
#11988 = FACE_OUTER_BOUND ( 'NONE', #10956, .T. ) ;
#11989 = CARTESIAN_POINT ( 'NONE',  ( 17.50000000000000355, 2.143131898507868643E-15, 40.00000000000000000 ) ) ;
#11990 = AXIS2_PLACEMENT_3D ( 'NONE', #11575, #6488, #3515 ) ;
#11991 = AXIS2_PLACEMENT_3D ( 'NONE', #14638, #116, #19508 ) ;
#11992 = CARTESIAN_POINT ( 'NONE',  ( 4.248408729364575365, -6.358192988180014993, -7.578543749819688813 ) ) ;
#11993 = DIRECTION ( 'NONE',  ( 0.000000000000000000, 0.000000000000000000, 1.000000000000000000 ) ) ;
#11994 = FILL_AREA_STYLE ('',( #16762 ) ) ;
#11995 = DIRECTION ( 'NONE',  ( 0.000000000000000000, 1.000000000000000000, -1.287488025362403787E-15 ) ) ;
#11996 = DIRECTION ( 'NONE',  ( -0.000000000000000000, -0.000000000000000000, 1.000000000000000000 ) ) ;
#11997 = ORIENTED_EDGE ( 'NONE', *, *, #6105, .F. ) ;
#11998 = CARTESIAN_POINT ( 'NONE',  ( -7.500000000000007105, 1.491842755816076505, 2.220731250087793818 ) ) ;
#11999 = ORIENTED_EDGE ( 'NONE', *, *, #2562, .T. ) ;
#12000 = CARTESIAN_POINT ( 'NONE',  ( -10.19618095047498052, 15.25966317163203101, 8.739106250180315172 ) ) ;
#12001 = DIRECTION ( 'NONE',  ( 0.000000000000000000, 0.000000000000000000, -1.000000000000000000 ) ) ;
#12002 = VERTEX_POINT ( 'NONE', #17555 ) ;
#12003 = EDGE_CURVE ( 'NONE', #17173, #17850, #20441, .T. ) ;
#12004 = DIRECTION ( 'NONE',  ( 0.000000000000000000, 0.000000000000000000, -1.000000000000000000 ) ) ;
#12005 = VERTEX_POINT ( 'NONE', #9478 ) ;
#12006 = CARTESIAN_POINT ( 'NONE',  ( 0.000000000000000000, -20.60847369612940128, -61.90898814327737654 ) ) ;
#12007 = DIRECTION ( 'NONE',  ( 1.000000000000000000, 0.000000000000000000, -0.000000000000000000 ) ) ;
#12008 = ADVANCED_FACE ( 'NONE', ( #17330 ), #20605, .F. ) ;
#12009 = ORIENTED_EDGE ( 'NONE', *, *, #9254, .F. ) ;
#12010 = DIRECTION ( 'NONE',  ( 0.000000000000000000, 0.000000000000000000, -1.000000000000000000 ) ) ;
#12011 = VECTOR ( 'NONE', #54, 1000.000000000000000 ) ;
#12012 = CARTESIAN_POINT ( 'NONE',  ( 5.200000000000002842, 0.000000000000000000, 0.000000000000000000 ) ) ;
#12013 = CARTESIAN_POINT ( 'NONE',  ( 6.888301784570727726, 16.62983158437509701, -18.06323749981969584 ) ) ;
#12014 = DIRECTION ( 'NONE',  ( -1.000000000000000000, -0.000000000000000000, -0.000000000000000000 ) ) ;
#12015 = CARTESIAN_POINT ( 'NONE',  ( 0.000000000000000000, 0.000000000000000000, 0.000000000000000000 ) ) ;
#12016 = CARTESIAN_POINT ( 'NONE',  ( -13.67243654642775041, 5.663308650141531508, -12.85122941848092815 ) ) ;
#12017 = CARTESIAN_POINT ( 'NONE',  ( 9.474249097082498849, -6.330490858644140850, 17.37620350064743135 ) ) ;
#12018 = EDGE_LOOP ( 'NONE', ( #10120, #11984, #17958, #4473 ) ) ;
#12019 = CARTESIAN_POINT ( 'NONE',  ( 19.99999999999999645, 3.141410481201071914, 65.17333458706188765 ) ) ;
#12020 = DIRECTION ( 'NONE',  ( 0.000000000000000000, 0.000000000000000000, -1.000000000000000000 ) ) ;
#12021 = ORIENTED_EDGE ( 'NONE', *, *, #18801, .T. ) ;
#12022 = CARTESIAN_POINT ( 'NONE',  ( 20.90734068544160351, -5.044436930659516705, -81.16927884214386779 ) ) ;
#12023 = VECTOR ( 'NONE', #7444, 1000.000000000000000 ) ;
#12024 = ORIENTED_EDGE ( 'NONE', *, *, #1193, .T. ) ;
#12025 = CARTESIAN_POINT ( 'NONE',  ( -6.888301780572501976, 16.62983158603122291, 1.513237500180310890 ) ) ;
#12026 = CARTESIAN_POINT ( 'NONE',  ( 19.99999999999999645, 63.17103598352149874, -16.33561182745074447 ) ) ;
#12027 = CARTESIAN_POINT ( 'NONE',  ( 19.99999999999999645, 67.51707036274447660, -25.00890260772307272 ) ) ;
#12028 = ORIENTED_EDGE ( 'NONE', *, *, #7435, .T. ) ;
#12029 = DIRECTION ( 'NONE',  ( -1.000000000000000000, 0.000000000000000000, 0.000000000000000000 ) ) ;
#12030 = ORIENTED_EDGE ( 'NONE', *, *, #18842, .F. ) ;
#12031 = DIRECTION ( 'NONE',  ( 0.000000000000000000, 0.000000000000000000, -1.000000000000000000 ) ) ;
#12032 = VERTEX_POINT ( 'NONE', #9584 ) ;
#12033 = CARTESIAN_POINT ( 'NONE',  ( -30.00000000000000000, -85.00000000000000000, -1.040949779275250179E-14 ) ) ;
#12034 = VECTOR ( 'NONE', #6066, 1000.000000000000000 ) ;
#12035 = ORIENTED_EDGE ( 'NONE', *, *, #18020, .F. ) ;
#12036 = CARTESIAN_POINT ( 'NONE',  ( 6.999999999999997335, 11.17999999999999972, 0.000000000000000000 ) ) ;
#12037 = EDGE_CURVE ( 'NONE', #6509, #9919, #2599, .T. ) ;
#12038 = AXIS2_PLACEMENT_3D ( 'NONE', #4992, #19399, #6569 ) ;
#12039 = PRODUCT ( 'socket head cap screw_iso_ISO 4762 M5 x 16 - 16N', 'socket head cap screw_iso_ISO 4762 M5 x 16 - 16N', '', ( #5048 ) ) ;
#12040 = CARTESIAN_POINT ( 'NONE',  ( 7.500000000000000000, 9.184850993605147944E-16, 166.0000000000000000 ) ) ;
#12041 = PRODUCT_CONTEXT ( 'NONE', #7078, 'mechanical' ) ;
#12042 = CARTESIAN_POINT ( 'NONE',  ( 14.79893867793684059, 2.943691925285398359, 15.44576066884154564 ) ) ;
#12043 = ORIENTED_EDGE ( 'NONE', *, *, #18120, .T. ) ;
#12044 = DIRECTION ( 'NONE',  ( 0.000000000000000000, 0.000000000000000000, -1.000000000000000000 ) ) ;
#12045 = VERTEX_POINT ( 'NONE', #17645 ) ;
#12046 = EDGE_CURVE ( 'NONE', #4233, #1822, #5891, .T. ) ;
#12047 = CARTESIAN_POINT ( 'NONE',  ( -21.03332064508573396, -4.547583584323819039, 88.88568648802799999 ) ) ;
#12048 =( GEOMETRIC_REPRESENTATION_CONTEXT ( 3 ) GLOBAL_UNCERTAINTY_ASSIGNED_CONTEXT ( ( #5804 ) ) GLOBAL_UNIT_ASSIGNED_CONTEXT ( ( #19495, #11757, #16618 ) ) REPRESENTATION_CONTEXT ( 'NONE', 'WORKASPACE' ) );
#12049 = CARTESIAN_POINT ( 'NONE',  ( -12.72792205982779556, 12.72792206288790773, 17.86957500018031197 ) ) ;
#12050 = CIRCLE ( 'NONE', #4276, 2.099999999999990763 ) ;
#12051 = DIRECTION ( 'NONE',  ( -6.938893903907228378E-17, 1.000000000000000000, -0.000000000000000000 ) ) ;
#12052 = AXIS2_PLACEMENT_3D ( 'NONE', #3345, #8421, #11499 ) ;
#12053 = CIRCLE ( 'NONE', #16453, 4.000000000000000888 ) ;
#12054 = ORIENTED_EDGE ( 'NONE', *, *, #10663, .F. ) ;
#12055 = DIRECTION ( 'NONE',  ( 0.000000000000000000, 0.000000000000000000, 1.000000000000000000 ) ) ;
#12056 = CARTESIAN_POINT ( 'NONE',  ( -0.6554360035617894376, 4.240386000424038571, -5.441324518471509997 ) ) ;
#12057 = VERTEX_POINT ( 'NONE', #17229 ) ;
#12058 = CARTESIAN_POINT ( 'NONE',  ( -3.788816106695048536, -22.69873778718781310, -75.50243859632158205 ) ) ;
#12059 = ORIENTED_EDGE ( 'NONE', *, *, #5336, .T. ) ;
#12060 = CARTESIAN_POINT ( 'NONE',  ( 45.22159793441012710, -8.673994507468391291, -90.00000000000001421 ) ) ;
#12061 = CARTESIAN_POINT ( 'NONE',  ( 17.99999999956957808, -3.580422614997675446, 12.27348125018031233 ) ) ;
#12062 = AXIS2_PLACEMENT_3D ( 'NONE', #2231, #18449, #11775 ) ;
#12063 = EDGE_LOOP ( 'NONE', ( #14280, #2300 ) ) ;
#12064 = ORIENTED_EDGE ( 'NONE', *, *, #20183, .T. ) ;
#12065 = FACE_OUTER_BOUND ( 'NONE', #9970, .T. ) ;
#12066 = EDGE_CURVE ( 'NONE', #7485, #17979, #4544, .T. ) ;
#12067 = AXIS2_PLACEMENT_3D ( 'NONE', #14836, #1701, #10059 ) ;
#12068 = EDGE_CURVE ( 'NONE', #15433, #11004, #15737, .T. ) ;
#12069 = FACE_BOUND ( 'NONE', #9172, .T. ) ;
#12070 = CARTESIAN_POINT ( 'NONE',  ( 3.599999999999909051, -10.82531754730554496, 129.0000000000000000 ) ) ;
#12071 = CARTESIAN_POINT ( 'NONE',  ( -17.50000000000000355, 0.000000000000000000, 46.00000000000000711 ) ) ;
#12072 = AXIS2_PLACEMENT_3D ( 'NONE', #7624, #966, #14207 ) ;
#12073 = VECTOR ( 'NONE', #20177, 1000.000000000000000 ) ;
#12075 = EDGE_CURVE ( 'NONE', #11798, #13280, #15703, .T. ) ;
#12074 = CARTESIAN_POINT ( 'NONE',  ( -54.64999999999999858, -39.99999999999999289, 5.000000000000000000 ) ) ;
#12076 = CARTESIAN_POINT ( 'NONE',  ( 5.303300858261588147, -5.303300859536636658, 7.816825000180313232 ) ) ;
#12077 = CARTESIAN_POINT ( 'NONE',  ( 7.500000000000007105, -1.491842755816074284, 16.35823125008779044 ) ) ;
#12078 = CARTESIAN_POINT ( 'NONE',  ( -6.330490856366290053, 9.474249098604506258, -12.71995350028680249 ) ) ;
#12079 = AXIS2_PLACEMENT_3D ( 'NONE', #20762, #17183, #19187 ) ;
#12080 = CARTESIAN_POINT ( 'NONE',  ( 19.99999999999999645, 70.68211945903208004, -13.71269443944133570 ) ) ;
#12081 = ORIENTED_EDGE ( 'NONE', *, *, #10013, .T. ) ;
#12082 = DIRECTION ( 'NONE',  ( 0.000000000000000000, 0.000000000000000000, 1.000000000000000000 ) ) ;
#12083 = AXIS2_PLACEMENT_3D ( 'NONE', #8429, #16586, #14904 ) ;
#12084 = CARTESIAN_POINT ( 'NONE',  ( -2.163827323447878234E-09, -18.00000000000000000, -12.03519999981969235 ) ) ;
#12085 = DIRECTION ( 'NONE',  ( 0.000000000000000000, 0.000000000000000000, 1.000000000000000000 ) ) ;
#12086 = EDGE_CURVE ( 'NONE', #9945, #2326, #4204, .T. ) ;
#12087 = ORIENTED_EDGE ( 'NONE', *, *, #14193, .T. ) ;
#12088 = EDGE_CURVE ( 'NONE', #2608, #19852, #11385, .T. ) ;
#12089 = DIRECTION ( 'NONE',  ( 0.000000000000000000, 0.000000000000000000, 1.000000000000000000 ) ) ;
#12090 = VECTOR ( 'NONE', #15649, 1000.000000000000000 ) ;
#12091 = VERTEX_POINT ( 'NONE', #1742 ) ;
#12092 = DIRECTION ( 'NONE',  ( 1.000000000000000000, 0.000000000000000000, 0.000000000000000000 ) ) ;
#12093 = DIRECTION ( 'NONE',  ( -1.000000000000000000, 0.000000000000000000, 0.000000000000000000 ) ) ;
#12094 = AXIS2_PLACEMENT_3D ( 'NONE', #7404, #9112, #16075 ) ;
#12095 = ORIENTED_EDGE ( 'NONE', *, *, #11428, .T. ) ;
#12096 = ORIENTED_EDGE ( 'NONE', *, *, #19713, .T. ) ;
#12097 = DIRECTION ( 'NONE',  ( 0.000000000000000000, 0.000000000000000000, -1.000000000000000000 ) ) ;
#12098 = EDGE_CURVE ( 'NONE', #8802, #10552, #7934, .T. ) ;
#12099 = CIRCLE ( 'NONE', #13799, 27.60000000002759890 ) ;
#12100 = FACE_OUTER_BOUND ( 'NONE', #15202, .T. ) ;
#12101 = CARTESIAN_POINT ( 'NONE',  ( -27.96694501150314593, -24.74873734152930993, -120.0000000000000142 ) ) ;
#12102 = VECTOR ( 'NONE', #4437, 1000.000000000000000 ) ;
#12103 = CARTESIAN_POINT ( 'NONE',  ( 7.499999999820660790, -1.491842756249031954, 0.6683312501803116978 ) ) ;
#12104 = CARTESIAN_POINT ( 'NONE',  ( 9.999999999999998224, -38.22257254261700155, -61.01667762370178139 ) ) ;
#12105 = CARTESIAN_POINT ( 'NONE',  ( 0.000000000000000000, -20.60847369613026103, 61.90898814327709943 ) ) ;
#12106 = LINE ( 'NONE', #18572, #3733 ) ;
#12107 = CARTESIAN_POINT ( 'NONE',  ( -49.35000000000000142, -39.99999999999999289, 5.000000000000000000 ) ) ;
#12108 = ORIENTED_EDGE ( 'NONE', *, *, #11968, .T. ) ;
#12109 = CARTESIAN_POINT ( 'NONE',  ( 30.00000000000000000, -97.49621075554985339, -111.6458212409894486 ) ) ;
#12110 = VERTEX_POINT ( 'NONE', #14872 ) ;
#12111 = CARTESIAN_POINT ( 'NONE',  ( 15.25966317163202746, 10.19618095047498407, 1.670356250180311752 ) ) ;
#12112 = CARTESIAN_POINT ( 'NONE',  ( -19.56401537842534921, -8.921674172384486567, 77.87798366923532001 ) ) ;
#12113 = ORIENTED_EDGE ( 'NONE', *, *, #13509, .T. ) ;
#12114 = DIRECTION ( 'NONE',  ( -0.000000000000000000, -0.000000000000000000, -1.000000000000000000 ) ) ;
#12115 = VERTEX_POINT ( 'NONE', #347 ) ;
#12116 = CARTESIAN_POINT ( 'NONE',  ( 45.41022184210711998, -126.8797397267199045, 84.49691278257978411 ) ) ;
#12117 = DIRECTION ( 'NONE',  ( -1.000000000000000000, 0.000000000000000000, 0.000000000000000000 ) ) ;
#12118 = CIRCLE ( 'NONE', #14463, 5.000000000000004441 ) ;
#12119 = ORIENTED_EDGE ( 'NONE', *, *, #11823, .F. ) ;
#12120 = FACE_OUTER_BOUND ( 'NONE', #16564, .T. ) ;
#12121 = DIRECTION ( 'NONE',  ( 1.000000000000000000, 0.000000000000000000, 0.000000000000000000 ) ) ;
#12122 = CARTESIAN_POINT ( 'NONE',  ( -10.19618095414378445, -15.25966316918061239, -3.631206249819690424 ) ) ;
#12123 = CARTESIAN_POINT ( 'NONE',  ( 17.50000000000000355, -2.143131898507868643E-15, -43.00000000000000000 ) ) ;
#12124 = PLANE ( 'NONE',  #16693 ) ;
#12125 = CARTESIAN_POINT ( 'NONE',  ( -2.222972771497745192, -11.17563879704982632, -18.55660899935256936 ) ) ;
#12126 = EDGE_LOOP ( 'NONE', ( #1188, #17426 ) ) ;
#12127 = SURFACE_SIDE_STYLE ('',( #20168 ) ) ;
#12128 = EDGE_CURVE ( 'NONE', #7832, #19785, #9949, .T. ) ;
#12129 = FACE_OUTER_BOUND ( 'NONE', #15851, .T. ) ;
#12130 = ORIENTED_EDGE ( 'NONE', *, *, #12195, .T. ) ;
#12131 = CARTESIAN_POINT ( 'NONE',  ( -19.81419003091921383, -8.351337688303459572, -78.32518794914258820 ) ) ;
#12132 = VERTEX_POINT ( 'NONE', #2041 ) ;
#12133 = CARTESIAN_POINT ( 'NONE',  ( -16.62983158603122291, -6.888301780572501087, -0.8430124998196862895 ) ) ;
#12134 = DIRECTION ( 'NONE',  ( -0.000000000000000000, -0.000000000000000000, -1.000000000000000000 ) ) ;
#12135 = LINE ( 'NONE', #17006, #5628 ) ;
#12136 = ORIENTED_EDGE ( 'NONE', *, *, #10229, .F. ) ;
#12137 = LINE ( 'NONE', #9830, #3148 ) ;
#12138 = ORIENTED_EDGE ( 'NONE', *, *, #20111, .F. ) ;
#12139 = CARTESIAN_POINT ( 'NONE',  ( 4.248408730893249441, 6.358192987158596488, 14.59104375018031519 ) ) ;
#12140 = EDGE_LOOP ( 'NONE', ( #12682, #2832 ) ) ;
#12141 = DIRECTION ( 'NONE',  ( 0.000000000000000000, 0.000000000000000000, 1.000000000000000000 ) ) ;
#12142 = CARTESIAN_POINT ( 'NONE',  ( 50.00000000000000000, -164.9999999999999716, -50.00000000000000711 ) ) ;
#12143 = DIRECTION ( 'NONE',  ( 0.000000000000000000, 0.000000000000000000, -1.000000000000000000 ) ) ;
#12144 = PRODUCT_CONTEXT ( 'NONE', #13591, 'mechanical' ) ;
#12145 = CARTESIAN_POINT ( 'NONE',  ( -10.46442989202484242, 10.46442989454075700, 2.780916918841545460 ) ) ;
#12146 = ORIENTED_EDGE ( 'NONE', *, *, #6765, .T. ) ;
#12147 = EDGE_CURVE ( 'NONE', #988, #15454, #8587, .T. ) ;
#12148 = CARTESIAN_POINT ( 'NONE',  ( 0.000000000000000000, 31.98952867950403345, -56.39803944231551469 ) ) ;
#12149 = ORIENTED_EDGE ( 'NONE', *, *, #12844, .F. ) ;
#12150 = CARTESIAN_POINT ( 'NONE',  ( -16.04895590985772458, -14.36624353526105402, 80.08463211907583457 ) ) ;
#12151 = CARTESIAN_POINT ( 'NONE',  ( 13.67243654778934925, 5.663308646854335215, -18.74185441848092637 ) ) ;
#12152 = FACE_BOUND ( 'NONE', #2183, .T. ) ;
#12153 = EDGE_CURVE ( 'NONE', #8902, #5012, #1168, .T. ) ;
#12154 = ORIENTED_EDGE ( 'NONE', *, *, #10485, .F. ) ;
#12155 = CARTESIAN_POINT ( 'NONE',  ( 31.47548550611441343, -112.5521019397693436, 80.04644125633257090 ) ) ;
#12156 = CYLINDRICAL_SURFACE ( 'NONE', #14488, 65.24900000006525147 ) ;
#12157 = ORIENTED_EDGE ( 'NONE', *, *, #10272, .T. ) ;
#12158 = CARTESIAN_POINT ( 'NONE',  ( 2.723238954207318319, -22.84144205494821023, -75.44116118571403717 ) ) ;
#12159 = VERTEX_POINT ( 'NONE', #3420 ) ;
#12160 = DIRECTION ( 'NONE',  ( 0.000000000000000000, 0.000000000000000000, 1.000000000000000000 ) ) ;
#12161 = CARTESIAN_POINT ( 'NONE',  ( 18.00000000043040771, 3.580422610670018546, 2.259418750180309576 ) ) ;
#12162 = ORIENTED_EDGE ( 'NONE', *, *, #8438, .T. ) ;
#12163 = ORIENTED_EDGE ( 'NONE', *, *, #10693, .T. ) ;
#12164 = CARTESIAN_POINT ( 'NONE',  ( 47.57345354676051130, -5.300163754693015150, -88.03325769612199281 ) ) ;
#12165 = FACE_OUTER_BOUND ( 'NONE', #1240, .T. ) ;
#12166 = DIRECTION ( 'NONE',  ( 0.000000000000000000, 0.000000000000000000, 1.000000000000000000 ) ) ;
#12167 = CARTESIAN_POINT ( 'NONE',  ( 8.500000000000000000, 1.040949779275250140E-15, -81.99999999999998579 ) ) ;
#12168 = SURFACE_SIDE_STYLE ('',( #15352 ) ) ;
#12169 = CARTESIAN_POINT ( 'NONE',  ( 9.015937996181842420E-10, 7.500000000000007994, -14.56754999981968446 ) ) ;
#12170 = AXIS2_PLACEMENT_3D ( 'NONE', #15331, #819, #20296 ) ;
#12171 = UNCERTAINTY_MEASURE_WITH_UNIT (LENGTH_MEASURE( 1.000000000000000082E-05 ), #234, 'distance_accuracy_value', 'NONE');
#12172 = CYLINDRICAL_SURFACE ( 'NONE', #3227, 7.500000000000000000 ) ;
#12173 = CARTESIAN_POINT ( 'NONE',  ( 6.929096493489630859, -2.870125743571144472, 7.227762500180316074 ) ) ;
#12174 = FACE_OUTER_BOUND ( 'NONE', #2376, .T. ) ;
#12175 = CARTESIAN_POINT ( 'NONE',  ( -7.902369978624323110, -7.902369976724391343, -24.79573475028681173 ) ) ;
#12176 = DIRECTION ( 'NONE',  ( 0.000000000000000000, 0.000000000000000000, 1.000000000000000000 ) ) ;
#12177 = ADVANCED_FACE ( 'NONE', ( #5110 ), #20920, .T. ) ;
#12178 = ORIENTED_EDGE ( 'NONE', *, *, #19706, .T. ) ;
#12179 = LINE ( 'NONE', #14102, #7524 ) ;
#12180 = EDGE_CURVE ( 'NONE', #1999, #13850, #8940, .T. ) ;
#12181 = CARTESIAN_POINT ( 'NONE',  ( -15.25966317163203279, -10.19618095047498052, -1.137543749819686978 ) ) ;
#12182 = CARTESIAN_POINT ( 'NONE',  ( -30.00000000000000000, -42.57363661491096707, -121.3828884801879155 ) ) ;
#12183 = EDGE_LOOP ( 'NONE', ( #18680, #13054, #16400, #2758 ) ) ;
#12184 = DIRECTION ( 'NONE',  ( -1.000000000000000000, 0.000000000000000000, 0.000000000000000000 ) ) ;
#12185 = ORIENTED_EDGE ( 'NONE', *, *, #8639, .T. ) ;
#12186 = DIRECTION ( 'NONE',  ( -1.000000000000000000, 0.000000000000000000, 0.000000000000000000 ) ) ;
#12187 = DIRECTION ( 'NONE',  ( -1.000000000000000000, 0.000000000000000000, 0.000000000000000000 ) ) ;
#12188 = ORIENTED_EDGE ( 'NONE', *, *, #10869, .F. ) ;
#12189 = EDGE_CURVE ( 'NONE', #14005, #18991, #6231, .T. ) ;
#12190 = VERTEX_POINT ( 'NONE', #18158 ) ;
#12191 = CARTESIAN_POINT ( 'NONE',  ( 3.599999999999913936, -10.82531754730554496, 166.0000000000000000 ) ) ;
#12192 =( NAMED_UNIT ( * ) PLANE_ANGLE_UNIT ( ) SI_UNIT ( $, .RADIAN. ) );
#12193 = DIRECTION ( 'NONE',  ( -0.000000000000000000, -1.000000000000000000, -0.000000000000000000 ) ) ;
#12194 = DIRECTION ( 'NONE',  ( -1.000000000000000000, -0.000000000000000000, 0.000000000000000000 ) ) ;
#12195 = EDGE_CURVE ( 'NONE', #10678, #6079, #6596, .T. ) ;
#12196 = CARTESIAN_POINT ( 'NONE',  ( -1.491842754445841246, 7.500000000179339210, -11.70198124981968846 ) ) ;
#12197 = CIRCLE ( 'NONE', #8132, 72.00000000007199219 ) ;
#12198 = DIRECTION ( 'NONE',  ( -1.000000000000000000, 0.000000000000000000, 0.000000000000000000 ) ) ;
#12199 = DIRECTION ( 'NONE',  ( 0.000000000000000000, -0.6310879443260593025, 0.7757112907044145800 ) ) ;
#12200 = CARTESIAN_POINT ( 'NONE',  ( 19.99999999999999645, 63.48283426024850229, 33.96954156735390740 ) ) ;
#12201 = DIRECTION ( 'NONE',  ( 0.000000000000000000, 0.000000000000000000, -1.000000000000000000 ) ) ;
#12202 = ADVANCED_FACE ( 'NONE', ( #19743 ), #3843, .F. ) ;
#12203 = CONICAL_SURFACE ( 'NONE', #14917, 4.000000000000000000, 1.047197551196595855 ) ;
#12204 = ORIENTED_EDGE ( 'NONE', *, *, #672, .T. ) ;
#12205 = FACE_OUTER_BOUND ( 'NONE', #8138, .T. ) ;
#12206 = EDGE_CURVE ( 'NONE', #10337, #7685, #4809, .T. ) ;
#12207 = ORIENTED_EDGE ( 'NONE', *, *, #12871, .F. ) ;
#12208 = CARTESIAN_POINT ( 'NONE',  ( -15.25966316918061771, 10.19618095414378622, 8.150043750180314461 ) ) ;
#12209 = CARTESIAN_POINT ( 'NONE',  ( -14.94551481348182165, -15.47228562136404584, 73.52041642655926523 ) ) ;
#12210 = AXIS2_PLACEMENT_3D ( 'NONE', #4692, #4372, #16029 ) ;
#12211 = ORIENTED_EDGE ( 'NONE', *, *, #15727, .T. ) ;
#12212 = FACE_OUTER_BOUND ( 'NONE', #12936, .T. ) ;
#12213 = ORIENTED_EDGE ( 'NONE', *, *, #11702, .T. ) ;
#12214 = EDGE_CURVE ( 'NONE', #896, #440, #6558, .T. ) ;
#12215 = PRODUCT_DEFINITION_SHAPE ( 'NONE', 'NONE',  #20953 ) ;
#12216 = LINE ( 'NONE', #7438, #1735 ) ;
#12217 = FACE_OUTER_BOUND ( 'NONE', #8384, .T. ) ;
#12218 = CARTESIAN_POINT ( 'NONE',  ( -6.232800000000000118, 1.325911618322048272E-15, -10.79377999999999993 ) ) ;
#12219 = ORIENTED_EDGE ( 'NONE', *, *, #12269, .T. ) ;
#12220 = FACE_BOUND ( 'NONE', #19261, .T. ) ;
#12221 = DIRECTION ( 'NONE',  ( -0.000000000000000000, -0.000000000000000000, -1.000000000000000000 ) ) ;
#12222 = CARTESIAN_POINT ( 'NONE',  ( 6.888301780572505528, -16.62983158603121581, -5.103862499819689980 ) ) ;
#12223 = CARTESIAN_POINT ( 'NONE',  ( -4.000000000000000000, 0.7862748000878172494, -5.565527722372433317 ) ) ;
#12224 = CARTESIAN_POINT ( 'NONE',  ( -7.500000000000000888, -3.289131931895657122E-15, 5.086300000002307087 ) ) ;
#12225 = AXIS2_PLACEMENT_3D ( 'NONE', #11363, #17839, #14642 ) ;
#12226 = CARTESIAN_POINT ( 'NONE',  ( 7.902369976724399336, -7.902369978624331104, -10.60426524935257042 ) ) ;
#12227 = ORIENTED_EDGE ( 'NONE', *, *, #6075, .F. ) ;
#12228 = EDGE_CURVE ( 'NONE', #12404, #7756, #11644, .T. ) ;
#12229 = FACE_OUTER_BOUND ( 'NONE', #9281, .T. ) ;
#12230 = EDGE_LOOP ( 'NONE', ( #4580, #5601, #9821, #1738 ) ) ;
#12231 = CARTESIAN_POINT ( 'NONE',  ( 9.482998254698379981, -19.29932845388887230, -71.54974094241291027 ) ) ;
#12232 = ORIENTED_EDGE ( 'NONE', *, *, #16816, .F. ) ;
#12233 = CARTESIAN_POINT ( 'NONE',  ( 16.62983158437509346, -6.888301784570739272, -13.80238749981968915 ) ) ;
#12234 = CARTESIAN_POINT ( 'NONE',  ( -24.99999999999999289, -42.57363661491096707, -121.3828884801879155 ) ) ;
#12235 = CYLINDRICAL_SURFACE ( 'NONE', #7325, 2.500000000000002220 ) ;
#12236 = AXIS2_PLACEMENT_3D ( 'NONE', #9953, #3293, #13044 ) ;
#12237 = ORIENTED_EDGE ( 'NONE', *, *, #15414, .T. ) ;
#12238 = CIRCLE ( 'NONE', #10926, 65.24900000006525147 ) ;
#12239 = FACE_OUTER_BOUND ( 'NONE', #12985, .T. ) ;
#12240 = ORIENTED_EDGE ( 'NONE', *, *, #10727, .F. ) ;
#12241 = FACE_OUTER_BOUND ( 'NONE', #1026, .T. ) ;
#12242 = CIRCLE ( 'NONE', #7497, 10.52399999999999380 ) ;
#12243 = ORIENTED_EDGE ( 'NONE', *, *, #14281, .F. ) ;
#12244 = EDGE_CURVE ( 'NONE', #12867, #14502, #1943, .T. ) ;
#12245 = PRESENTATION_LAYER_ASSIGNMENT (  '', '', ( #20343 ) ) ;
#12246 = DIRECTION ( 'NONE',  ( 1.000000000000000000, 0.000000000000000000, 0.000000000000000000 ) ) ;
#12247 = DIRECTION ( 'NONE',  ( -1.000000000000000000, -0.000000000000000000, -0.000000000000000000 ) ) ;
#12248 = CARTESIAN_POINT ( 'NONE',  ( 14.79893867722910450, -2.943691928843438443, -2.815176831158457293 ) ) ;
#12249 = VECTOR ( 'NONE', #7363, 1000.000000000000000 ) ;
#12251 = VERTEX_POINT ( 'NONE', #5021 ) ;
#12250 = VECTOR ( 'NONE', #19506, 1000.000000000000000 ) ;
#12252 = DIRECTION ( 'NONE',  ( -1.000000000000000000, -0.000000000000000000, 0.000000000000000000 ) ) ;
#12253 = AXIS2_PLACEMENT_3D ( 'NONE', #8054, #14422, #11226 ) ;
#12254 = ORIENTED_EDGE ( 'NONE', *, *, #17922, .T. ) ;
#12255 = CARTESIAN_POINT ( 'NONE',  ( -19.10408208028293586, -9.878941057108505674, 83.54765472770249346 ) ) ;
#12256 = CARTESIAN_POINT ( 'NONE',  ( 17.99999999999999645, -2.163824016901520184E-09, 2.553950000180309932 ) ) ;
#12257 = CARTESIAN_POINT ( 'NONE',  ( -7.500000000000004441, 9.706494107352906755E-15, -23.18869999999769860 ) ) ;
#12258 = DIRECTION ( 'NONE',  ( 0.000000000000000000, 0.000000000000000000, 1.000000000000000000 ) ) ;
#12259 = VERTEX_POINT ( 'NONE', #17754 ) ;
#12260 = DIRECTION ( 'NONE',  ( -1.597351267013635531E-16, 1.000000000000000000, 0.000000000000000000 ) ) ;
#12261 = CARTESIAN_POINT ( 'NONE',  ( 6.232799999999998342, 9.267171751443831555E-16, -7.567219999999999835 ) ) ;
#12262 = ORIENTED_EDGE ( 'NONE', *, *, #8097, .F. ) ;
#12263 = VECTOR ( 'NONE', #14198, 1000.000000000000000 ) ;
#12264 = DIRECTION ( 'NONE',  ( -1.000000000000000000, -0.000000000000000000, -0.000000000000000000 ) ) ;
#12265 = EDGE_CURVE ( 'NONE', #16773, #6425, #9283, .T. ) ;
#12266 = AXIS2_PLACEMENT_3D ( 'NONE', #6678, #17276, #18553 ) ;
#12267 = ORIENTED_EDGE ( 'NONE', *, *, #4019, .T. ) ;
#12268 = CARTESIAN_POINT ( 'NONE',  ( -6.888301780572500199, 16.62983158603121936, -19.24136249981969016 ) ) ;
#12269 = EDGE_CURVE ( 'NONE', #857, #3130, #134, .T. ) ;
#12270 = VECTOR ( 'NONE', #19580, 1000.000000000000000 ) ;
#12271 = ORIENTED_EDGE ( 'NONE', *, *, #3009, .T. ) ;
#12272 = VECTOR ( 'NONE', #8553, 1000.000000000000000 ) ;
#12273 = ORIENTED_EDGE ( 'NONE', *, *, #13538, .F. ) ;
#12274 = DIRECTION ( 'NONE',  ( 1.000000000000000000, 0.000000000000000000, 0.000000000000000000 ) ) ;
#12275 = DIRECTION ( 'NONE',  ( -0.000000000000000000, -0.000000000000000000, -1.000000000000000000 ) ) ;
#12276 = DIRECTION ( 'NONE',  ( 0.000000000000000000, -0.1361666490962331333, -0.9906859460363326431 ) ) ;
#12277 = DIRECTION ( 'NONE',  ( 0.000000000000000000, 0.2697967711570183891, 0.9629172873478009098 ) ) ;
#12278 =( NAMED_UNIT ( * ) PLANE_ANGLE_UNIT ( ) SI_UNIT ( $, .RADIAN. ) );
#12279 = VECTOR ( 'NONE', #13329, 1000.000000000000000 ) ;
#12280 = CARTESIAN_POINT ( 'NONE',  ( -12.72792206288791483, -12.72792205982780089, -1.432074999819690664 ) ) ;
#12281 = CARTESIAN_POINT ( 'NONE',  ( 7.000000000000000000, 11.17999999999999972, 0.000000000000000000 ) ) ;
#12282 = EDGE_LOOP ( 'NONE', ( #12624, #1543 ) ) ;
#12283 = CIRCLE ( 'NONE', #20039, 27.60000000002760245 ) ;
#12284 = DIRECTION ( 'NONE',  ( 0.000000000000000000, 0.000000000000000000, -1.000000000000000000 ) ) ;
#12285 = VECTOR ( 'NONE', #5159, 1000.000000000000000 ) ;
#12286 = CARTESIAN_POINT ( 'NONE',  ( -2.943691925285395694, 14.79893867793683349, 16.89642683151907576 ) ) ;
#12287 = MECHANICAL_DESIGN_GEOMETRIC_PRESENTATION_REPRESENTATION (  '', ( #18720 ), #8547 ) ;
#12288 = AXIS2_PLACEMENT_3D ( 'NONE', #13319, #6731, #13525 ) ;
#12289 = CARTESIAN_POINT ( 'NONE',  ( -27.96694501150314593, -24.74873734152930993, -120.0000000000000142 ) ) ;
#12290 = VERTEX_POINT ( 'NONE', #14572 ) ;
#12291 = CYLINDRICAL_SURFACE ( 'NONE', #4824, 65.24900000006525147 ) ;
#12292 = CARTESIAN_POINT ( 'NONE',  ( 1.040949779275250179E-14, -85.00000000000000000, 19.00000000000000000 ) ) ;
#12293 = DIRECTION ( 'NONE',  ( 1.000000000000000000, 0.000000000000000000, 0.000000000000000000 ) ) ;
#12294 = AXIS2_PLACEMENT_3D ( 'NONE', #20601, #10763, #11074 ) ;
#12295 = ORIENTED_EDGE ( 'NONE', *, *, #3259, .F. ) ;
#12296 = AXIS2_PLACEMENT_3D ( 'NONE', #8791, #11875, #8699 ) ;
#12297 = DIRECTION ( 'NONE',  ( 1.000000000000000000, 0.000000000000000000, 0.000000000000000000 ) ) ;
#12298 = EDGE_LOOP ( 'NONE', ( #2463, #18389, #20453, #1995 ) ) ;
#12299 = LINE ( 'NONE', #4351, #5782 ) ;
#12300 = DIRECTION ( 'NONE',  ( 0.000000000000000000, 0.000000000000000000, 1.000000000000000000 ) ) ;
#12301 = ORIENTED_EDGE ( 'NONE', *, *, #19682, .T. ) ;
#12302 = ORIENTED_EDGE ( 'NONE', *, *, #4704, .F. ) ;
#12303 = DIRECTION ( 'NONE',  ( -0.000000000000000000, -0.000000000000000000, 1.000000000000000000 ) ) ;
#12304 = CIRCLE ( 'NONE', #7201, 35.00000000000000000 ) ;
#12305 = CIRCLE ( 'NONE', #5506, 65.24900000006525147 ) ;
#12306 = DIRECTION ( 'NONE',  ( 0.000000000000000000, -0.000000000000000000, 1.000000000000000000 ) ) ;
#12307 = EDGE_CURVE ( 'NONE', #1037, #12032, #17412, .T. ) ;
#12308 = EDGE_CURVE ( 'NONE', #4610, #12350, #8267, .T. ) ;
#12309 = CARTESIAN_POINT ( 'NONE',  ( 19.99999999999999645, 46.01927912072591198, -45.67597560296339765 ) ) ;
#12310 = VECTOR ( 'NONE', #16764, 1000.000000000000000 ) ;
#12311 = VECTOR ( 'NONE', #19697, 1000.000000000000000 ) ;
#12312 = CARTESIAN_POINT ( 'NONE',  ( -2.870125741905209971, 6.929096494179676213, -11.99651249981969059 ) ) ;
#12313 = CARTESIAN_POINT ( 'NONE',  ( 50.00000000000000000, -42.57363661491096707, -71.38288848018790134 ) ) ;
#12314 = CIRCLE ( 'NONE', #13004, 2.649999999999993694 ) ;
#12315 = DIRECTION ( 'NONE',  ( -1.000000000000000000, 0.000000000000000000, 0.000000000000000000 ) ) ;
#12316 = LINE ( 'NONE', #7644, #7982 ) ;
#12317 = EDGE_CURVE ( 'NONE', #5157, #3526, #13692, .T. ) ;
#12318 = AXIS2_PLACEMENT_3D ( 'NONE', #6779, #20127, #3911 ) ;
#12319 = AXIS2_PLACEMENT_3D ( 'NONE', #7358, #15623, #12785 ) ;
#12320 = ORIENTED_EDGE ( 'NONE', *, *, #12819, .T. ) ;
#12321 = DIRECTION ( 'NONE',  ( 0.000000000000000000, 0.000000000000000000, -1.000000000000000000 ) ) ;
#12322 = ORIENTED_EDGE ( 'NONE', *, *, #6009, .F. ) ;
#12323 = CARTESIAN_POINT ( 'NONE',  ( 18.00000000000000000, -2.163824016901520184E-09, 2.553950000180313484 ) ) ;
#12324 = FACE_OUTER_BOUND ( 'NONE', #18313, .T. ) ;
#12325 = ORIENTED_EDGE ( 'NONE', *, *, #4138, .T. ) ;
#12326 = CARTESIAN_POINT ( 'NONE',  ( 6.680000000000000604, -11.49999999999998757, 1.408343819019455584E-15 ) ) ;
#12327 = ORIENTED_EDGE ( 'NONE', *, *, #9057, .T. ) ;
#12328 = CARTESIAN_POINT ( 'NONE',  ( 45.02826274242529081, -126.4302678889703202, 84.01931467314857116 ) ) ;
#12329 = DIRECTION ( 'NONE',  ( -1.000000000000000000, -0.000000000000000000, -0.000000000000000000 ) ) ;
#12330 = DIRECTION ( 'NONE',  ( 0.000000000000000000, 0.000000000000000000, 1.000000000000000000 ) ) ;
#12331 = AXIS2_PLACEMENT_3D ( 'NONE', #9151, #17430, #20907 ) ;
#12332 = ORIENTED_EDGE ( 'NONE', *, *, #12480, .T. ) ;
#12333 = LINE ( 'NONE', #18799, #2571 ) ;
#12334 = CIRCLE ( 'NONE', #4506, 72.00000000007199219 ) ;
#12335 = CARTESIAN_POINT ( 'NONE',  ( 47.57345354676048998, -5.300163754693023144, 88.03325769612197860 ) ) ;
#12336 = CARTESIAN_POINT ( 'NONE',  ( -10.19618095047497874, 15.25966317163202746, -19.53589374981968874 ) ) ;
#12337 = CARTESIAN_POINT ( 'NONE',  ( 49.19234958605026264, -1.326995226329893862, 84.99999999999998579 ) ) ;
#12338 = EDGE_CURVE ( 'NONE', #11557, #8862, #766, .T. ) ;
#12339 = CIRCLE ( 'NONE', #7232, 2.649999999999987477 ) ;
#12340 = EDGE_CURVE ( 'NONE', #10176, #6274, #18429, .T. ) ;
#12341 = CARTESIAN_POINT ( 'NONE',  ( 1.491842754445842578, -7.500000000179340987, 11.86051875018030977 ) ) ;
#12342 = ORIENTED_EDGE ( 'NONE', *, *, #4404, .F. ) ;
#12343 = FILL_AREA_STYLE_COLOUR ( '', #10319 ) ;
#12344 = EDGE_CURVE ( 'NONE', #8735, #8470, #5417, .T. ) ;
#12345 = CYLINDRICAL_SURFACE ( 'NONE', #3713, 72.00000000007199219 ) ;
#12346 = EDGE_LOOP ( 'NONE', ( #13266, #7118, #17134, #17565 ) ) ;
#12347 = AXIS2_PLACEMENT_3D ( 'NONE', #25, #19728, #11672 ) ;
#12348 = CARTESIAN_POINT ( 'NONE',  ( 19.99999999999999645, 38.69327817041775575, 52.53819777490647880 ) ) ;
#12349 = CARTESIAN_POINT ( 'NONE',  ( -4.248408729364580694, 6.358192988180020322, -6.026143749819683038 ) ) ;
#12350 = VERTEX_POINT ( 'NONE', #2356 ) ;
#12351 = CARTESIAN_POINT ( 'NONE',  ( 2.163825119083639534E-09, 18.00000000000000000, -16.74769999981968738 ) ) ;
#12352 = CARTESIAN_POINT ( 'NONE',  ( 0.000000000000000000, 61.72688495901613948, -19.84591825364033468 ) ) ;
#12353 = CARTESIAN_POINT ( 'NONE',  ( 3.600000000000060485, 10.82531754730546147, 169.0000000000000000 ) ) ;
#12354 = ORIENTED_EDGE ( 'NONE', *, *, #127, .T. ) ;
#12355 = DIRECTION ( 'NONE',  ( -0.000000000000000000, -0.000000000000000000, 1.000000000000000000 ) ) ;
#12356 = ORIENTED_EDGE ( 'NONE', *, *, #2631, .T. ) ;
#12357 = AXIS2_PLACEMENT_3D ( 'NONE', #20675, #2678, #17204 ) ;
#12358 = CARTESIAN_POINT ( 'NONE',  ( 24.99999999999999645, -110.0000000000000142, -45.00000000000000711 ) ) ;
#12359 = B_SPLINE_CURVE_WITH_KNOTS ( 'NONE', 3,
 ( #15684, #13890, #11020, #11128, #17497, #9530, #1186, #6041, #18977, #12514, #20335, #7629, #10915, #14109, #20563, #4447, #17390, #3178, #15999, #19488, #16210, #1794 ),
 .UNSPECIFIED., .F., .F.,
 ( 4, 2, 2, 2, 2, 2, 2, 2, 2, 2, 4 ),
 ( 0.007433635558789152172, 0.01246066521146292627, 0.01497418003779982937, 0.01748769486413673246, 0.02754175416948434832, 0.03005526899582125142, 0.03256878382215815798, 0.03759581347483195030, 0.04262284312750573567, 0.04513635795384261795, 0.04764987278017949329 ),
 .UNSPECIFIED. ) ;
#12360 = EDGE_CURVE ( 'NONE', #3206, #17908, #8662, .T. ) ;
#12361 = ORIENTED_EDGE ( 'NONE', *, *, #15051, .F. ) ;
#12362 = EDGE_CURVE ( 'NONE', #17067, #16258, #151, .T. ) ;
#12363 = CARTESIAN_POINT ( 'NONE',  ( 30.25309211476868398, -108.6363473640507920, 73.18580831706346146 ) ) ;
#12364 = ADVANCED_FACE ( 'NONE', ( #10741 ), #4469, .T. ) ;
#12365 = LINE ( 'NONE', #17021, #7541 ) ;
#12366 = CONTEXT_DEPENDENT_SHAPE_REPRESENTATION ( #10633, #4074 ) ;
#12367 = CARTESIAN_POINT ( 'NONE',  ( -14.79893867758297610, 1.779018419858781159E-09, 1.602791918841543595 ) ) ;
#12368 = ORIENTED_EDGE ( 'NONE', *, *, #17213, .T. ) ;
#12369 = LINE ( 'NONE', #10779, #16002 ) ;
#12370 = ORIENTED_EDGE ( 'NONE', *, *, #14999, .T. ) ;
#12371 = CARTESIAN_POINT ( 'NONE',  ( -18.83539447212728390, -10.38388837219175542, 83.11735093927855189 ) ) ;
#12372 = CARTESIAN_POINT ( 'NONE',  ( 17.99999999956957808, -3.580422614997675446, 2.848481250180310287 ) ) ;
#12373 = CARTESIAN_POINT ( 'NONE',  ( 0.000000000000000000, 0.000000000000000000, 40.00000000000000000 ) ) ;
#12374 = DIRECTION ( 'NONE',  ( 0.000000000000000000, 0.000000000000000000, 1.000000000000000000 ) ) ;
#12375 = ORIENTED_EDGE ( 'NONE', *, *, #6455, .F. ) ;
#12376 = DIRECTION ( 'NONE',  ( 1.000000000000000000, 0.000000000000000000, 0.000000000000000000 ) ) ;
#12377 = FACE_BOUND ( 'NONE', #8872, .T. ) ;
#12378 = ORIENTED_EDGE ( 'NONE', *, *, #18666, .T. ) ;
#12379 = DIRECTION ( 'NONE',  ( -1.000000000000000000, -0.000000000000000000, -0.000000000000000000 ) ) ;
#12380 = VECTOR ( 'NONE', #19013, 1000.000000000000000 ) ;
#12381 = DIRECTION ( 'NONE',  ( 1.000000000000000000, 0.000000000000000000, 0.000000000000000000 ) ) ;
#12382 = CARTESIAN_POINT ( 'NONE',  ( 6.888301784570727726, 16.62983158437509701, -8.638237499819693355 ) ) ;
#12383 = SHAPE_REPRESENTATION ( 'socket head cap screw_iso_ISO 4762 M5 x 16 - 16N', ( #12461 ), #2587 ) ;
#12384 = ORIENTED_EDGE ( 'NONE', *, *, #16346, .F. ) ;
#12385 = CARTESIAN_POINT ( 'NONE',  ( 10.00000000000000178, -164.9999999999999716, 70.00000000000000000 ) ) ;
#12386 = DIRECTION ( 'NONE',  ( -1.000000000000000000, 0.000000000000000000, 0.000000000000000000 ) ) ;
#12387 = DIRECTION ( 'NONE',  ( 0.000000000000000000, 0.000000000000000000, 1.000000000000000000 ) ) ;
#12388 = CARTESIAN_POINT ( 'NONE',  ( 19.99999999999999645, -48.70996102988652154, -42.79495875147824790 ) ) ;
#12389 = CARTESIAN_POINT ( 'NONE',  ( 15.25966316918061771, -10.19618095414378800, 14.76714375018030978 ) ) ;
#12390 = UNCERTAINTY_MEASURE_WITH_UNIT (LENGTH_MEASURE( 1.000000000000000082E-05 ), #1927, 'distance_accuracy_value', 'NONE');
#12391 = VECTOR ( 'NONE', #2725, 1000.000000000000114 ) ;
#12392 = CARTESIAN_POINT ( 'NONE',  ( -6.358192987158596488, 4.248408730893249441, -16.04020624981968979 ) ) ;
#12393 = ORIENTED_EDGE ( 'NONE', *, *, #18959, .F. ) ;
#12394 = CARTESIAN_POINT ( 'NONE',  ( -7.500000000000007994, -4.022542210876018231E-17, 20.77620000000231570 ) ) ;
#12395 = VECTOR ( 'NONE', #20417, 1000.000000000000000 ) ;
#12396 = CARTESIAN_POINT ( 'NONE',  ( -14.79893867722910095, 2.943691928843434891, 5.704239331519073808 ) ) ;
#12397 = PRODUCT_DEFINITION_SHAPE ( 'NONE', 'NONE',  #20948 ) ;
#12398 = EDGE_CURVE ( 'NONE', #798, #7823, #20788, .T. ) ;
#12399 = DIRECTION ( 'NONE',  ( -1.000000000000000000, -0.000000000000000000, 0.000000000000000000 ) ) ;
#12400 = ORIENTED_EDGE ( 'NONE', *, *, #14421, .F. ) ;
#12401 = CARTESIAN_POINT ( 'NONE',  ( -7.500000000000009770, 9.706494115329868228E-15, -7.498799999997683763 ) ) ;
#12402 = CARTESIAN_POINT ( 'NONE',  ( -15.25966317163203279, -10.19618095047498052, -19.98754374981969306 ) ) ;
#12403 = DIRECTION ( 'NONE',  ( 0.000000000000000000, 0.000000000000000000, 1.000000000000000000 ) ) ;
#12404 = VERTEX_POINT ( 'NONE', #5846 ) ;
#12405 = DIRECTION ( 'NONE',  ( -1.000000000000000000, 0.000000000000000000, 0.000000000000000000 ) ) ;
#12406 = ORIENTED_EDGE ( 'NONE', *, *, #18404, .T. ) ;
#12407 = DIRECTION ( 'NONE',  ( 1.000000000000000000, 0.000000000000000000, 0.000000000000000000 ) ) ;
#12408 = DIRECTION ( 'NONE',  ( 0.000000000000000000, -0.9976687691905398170, 0.06824241336466078944 ) ) ;
#12409 = VECTOR ( 'NONE', #1925, 1000.000000000000000 ) ;
#12410 = VERTEX_POINT ( 'NONE', #14230 ) ;
#12411 = ORIENTED_EDGE ( 'NONE', *, *, #14490, .F. ) ;
#12412 = CYLINDRICAL_SURFACE ( 'NONE', #16468, 27.60000000002759535 ) ;
#12413 = CIRCLE ( 'NONE', #9371, 65.24900000006525147 ) ;
#12414 = VECTOR ( 'NONE', #6211, 1000.000000000000000 ) ;
#12415 = DIRECTION ( 'NONE',  ( 0.5017436386064966225, -6.031582975246074897E-11, 0.8650163704334810078 ) ) ;
#12416 = CIRCLE ( 'NONE', #6312, 7.500000000000000000 ) ;
#12417 = PLANE ( 'NONE',  #13940 ) ;
#12418 = AXIS2_PLACEMENT_3D ( 'NONE', #7178, #17161, #13659 ) ;
#12419 = CARTESIAN_POINT ( 'NONE',  ( 4.248408729364575365, -6.358192988180014993, -26.42854374981969201 ) ) ;
#12420 = EDGE_CURVE ( 'NONE', #18257, #15415, #10666, .T. ) ;
#12421 = AXIS2_PLACEMENT_3D ( 'NONE', #2413, #835, #8666 ) ;
#12422 = DIRECTION ( 'NONE',  ( -0.000000000000000000, -0.000000000000000000, 1.000000000000000000 ) ) ;
#12423 = FACE_BOUND ( 'NONE', #2786, .T. ) ;
#12424 = LINE ( 'NONE', #5840, #20842 ) ;
#12425 = CIRCLE ( 'NONE', #10394, 7.500000000000000000 ) ;
#12426 = ORIENTED_EDGE ( 'NONE', *, *, #19628, .F. ) ;
#12427 = LINE ( 'NONE', #2774, #11568 ) ;
#12428 = VERTEX_POINT ( 'NONE', #15596 ) ;
#12429 = CARTESIAN_POINT ( 'NONE',  ( -6.888301784570738384, -16.62983158437509346, -22.77573749981968732 ) ) ;
#12430 = DIRECTION ( 'NONE',  ( -1.000000000000000000, 0.000000000000000000, 0.000000000000000000 ) ) ;
#12431 = VERTEX_POINT ( 'NONE', #6269 ) ;
#12432 = EDGE_CURVE ( 'NONE', #5100, #12774, #6920, .T. ) ;
#12433 = CARTESIAN_POINT ( 'NONE',  ( -31.75000000000000000, 10.52399999999999558, 0.000000000000000000 ) ) ;
#12434 = VERTEX_POINT ( 'NONE', #7650 ) ;
#12435 = CARTESIAN_POINT ( 'NONE',  ( -7.500000000000004441, 9.706494107352906755E-15, -4.338699999997692736 ) ) ;
#12436 = DIRECTION ( 'NONE',  ( 1.000000000000000000, 0.000000000000000000, 0.000000000000000000 ) ) ;
#12437 = LINE ( 'NONE', #4269, #9706 ) ;
#12438 = AXIS2_PLACEMENT_3D ( 'NONE', #6350, #4969, #14721 ) ;
#12439 = ORIENTED_EDGE ( 'NONE', *, *, #11817, .F. ) ;
#12440 = DIRECTION ( 'NONE',  ( 0.000000000000000000, 0.9422609221188213979, -0.3348796121709836648 ) ) ;
#12441 = DIRECTION ( 'NONE',  ( 1.000000000000000000, 0.000000000000000000, 0.000000000000000000 ) ) ;
#12442 = CARTESIAN_POINT ( 'NONE',  ( -12.50000000000000533, 0.000000000000000000, 169.0000000000000000 ) ) ;
#12443 = CARTESIAN_POINT ( 'NONE',  ( 19.99999999999999645, 51.81019761368373366, -38.98425606966007706 ) ) ;
#12444 = CIRCLE ( 'NONE', #17538, 65.24900000006525147 ) ;
#12445 = AXIS2_PLACEMENT_3D ( 'NONE', #11242, #9957, #1812 ) ;
#12446 = CARTESIAN_POINT ( 'NONE',  ( 7.500000000000000888, -2.290195989456150567E-15, 9.798800000002307442 ) ) ;
#12447 = ORIENTED_EDGE ( 'NONE', *, *, #1219, .T. ) ;
#12448 = FACE_OUTER_BOUND ( 'NONE', #17394, .T. ) ;
#12449 = DIRECTION ( 'NONE',  ( 0.000000000000000000, 0.000000000000000000, 1.000000000000000000 ) ) ;
#12450 = ORIENTED_EDGE ( 'NONE', *, *, #11314, .F. ) ;
#12451 = AXIS2_PLACEMENT_3D ( 'NONE', #3528, #14984, #7918 ) ;
#12452 = DIRECTION ( 'NONE',  ( -1.000000000000000000, -0.000000000000000000, 0.000000000000000000 ) ) ;
#12453 = LINE ( 'NONE', #17225, #7552 ) ;
#12454 = ORIENTED_EDGE ( 'NONE', *, *, #5729, .F. ) ;
#12455 = AXIS2_PLACEMENT_3D ( 'NONE', #17561, #6303, #12886 ) ;
#12456 = CARTESIAN_POINT ( 'NONE',  ( -2.163827323447878234E-09, -18.00000000000000000, -21.46019999981968951 ) ) ;
#12457 = CARTESIAN_POINT ( 'NONE',  ( 30.00000000000000000, -39.99999999999999289, 49.90000000000000568 ) ) ;
#12458 = DIRECTION ( 'NONE',  ( 0.000000000000000000, 0.000000000000000000, -1.000000000000000000 ) ) ;
#12459 = VERTEX_POINT ( 'NONE', #6159 ) ;
#12460 = EDGE_CURVE ( 'NONE', #939, #9908, #5952, .T. ) ;
#12461 = AXIS2_PLACEMENT_3D ( 'NONE', #19474, #3361, #185 ) ;
#12462 = CARTESIAN_POINT ( 'NONE',  ( 8.900000000000046541, 10.82531754730546147, 166.0000000000000000 ) ) ;
#12463 = VERTEX_POINT ( 'NONE', #12756 ) ;
#12464 = CARTESIAN_POINT ( 'NONE',  ( 29.99999999999965183, -164.9999999999999716, -50.00000000000002842 ) ) ;
#12465 = EDGE_CURVE ( 'NONE', #20215, #4706, #13363, .T. ) ;
#12466 = ORIENTED_EDGE ( 'NONE', *, *, #668, .F. ) ;
#12467 = EDGE_CURVE ( 'NONE', #12002, #10263, #9245, .T. ) ;
#12468 = EDGE_CURVE ( 'NONE', #18656, #4973, #16073, .T. ) ;
#12469 = CARTESIAN_POINT ( 'NONE',  ( 31.27523735953079864, -112.0413217638139827, 74.38135980682834258 ) ) ;
#12470 = PRODUCT_RELATED_PRODUCT_CATEGORY ( 'part', '', ( #6770 ) ) ;
#12471 = CARTESIAN_POINT ( 'NONE',  ( -10.46442989454075878, -10.46442989202484242, -9.000333081158460757 ) ) ;
#12472 = ORIENTED_EDGE ( 'NONE', *, *, #20293, .F. ) ;
#12473 = DIRECTION ( 'NONE',  ( 0.000000000000000000, 0.000000000000000000, 1.000000000000000000 ) ) ;
#12474 = ORIENTED_EDGE ( 'NONE', *, *, #3400, .T. ) ;
#12475 = CARTESIAN_POINT ( 'NONE',  ( 18.21773432164967232, -11.43289491867056817, 82.25893718214402384 ) ) ;
#12476 = ADVANCED_FACE ( 'NONE', ( #12324 ), #19441, .T. ) ;
#12477 = CARTESIAN_POINT ( 'NONE',  ( 16.62983158437509346, -6.888301784570737496, 3.143012500180311086 ) ) ;
#12478 = CARTESIAN_POINT ( 'NONE',  ( 9.015937996181835182E-10, 7.500000000000002665, -20.83244999981969059 ) ) ;
#12479 = DIRECTION ( 'NONE',  ( 1.000000000000000000, -0.000000000000000000, -0.000000000000000000 ) ) ;
#12480 = EDGE_CURVE ( 'NONE', #9722, #8274, #14027, .T. ) ;
#12481 = ORIENTED_EDGE ( 'NONE', *, *, #1529, .T. ) ;
#12482 = EDGE_CURVE ( 'NONE', #17420, #5525, #17617, .T. ) ;
#12483 = CARTESIAN_POINT ( 'NONE',  ( 19.99999999999999645, -27.62776854598816101, -58.65812137499030854 ) ) ;
#12484 = CARTESIAN_POINT ( 'NONE',  ( 30.00000000000000355, -139.6410161513775563, 90.00000000000001421 ) ) ;
#12485 = CONICAL_SURFACE ( 'NONE', #17903, 4.000000000000000000, 1.047197551196595855 ) ;
#12486 = ORIENTED_EDGE ( 'NONE', *, *, #11817, .T. ) ;
#12487 = CARTESIAN_POINT ( 'NONE',  ( 19.58689223458519990, -12.07292356518670395, -81.75718538670371061 ) ) ;
#12488 = CARTESIAN_POINT ( 'NONE',  ( -6.358192988180015881, -4.248408729364577141, 4.202706250180307634 ) ) ;
#12489 = EDGE_CURVE ( 'NONE', #18834, #4546, #6058, .T. ) ;
#12490 = CARTESIAN_POINT ( 'NONE',  ( -18.00000000043040771, -3.580422610670021211, -11.87808124981969193 ) ) ;
#12491 = EDGE_CURVE ( 'NONE', #833, #15651, #503, .T. ) ;
#12492 = ORIENTED_EDGE ( 'NONE', *, *, #7392, .F. ) ;
#12493 = DIRECTION ( 'NONE',  ( 1.000000000000000000, 0.000000000000000000, 0.000000000000000000 ) ) ;
#12494 = DIRECTION ( 'NONE',  ( 0.000000000000000000, -0.8878852184023702243, -0.4600650377311618633 ) ) ;
#12495 = DIRECTION ( 'NONE',  ( -1.000000000000000000, -0.000000000000000000, -0.000000000000000000 ) ) ;
#12496 = CARTESIAN_POINT ( 'NONE',  ( 0.000000000000000000, 1.971042061628357933, 64.80882494896107460 ) ) ;
#12497 = DIRECTION ( 'NONE',  ( -7.888609052210117178E-31, 1.577721810442023260E-30, -1.000000000000000000 ) ) ;
#12498 = CARTESIAN_POINT ( 'NONE',  ( 15.25966317163203101, 10.19618095047498585, 3.574956250180307826 ) ) ;
#12499 = CARTESIAN_POINT ( 'NONE',  ( 6.929096493489630859, -2.870125743571144472, -11.62223749981968624 ) ) ;
#12500 = VERTEX_POINT ( 'NONE', #6466 ) ;
#12501 = CIRCLE ( 'NONE', #3672, 27.60000000002759535 ) ;
#12502 = CARTESIAN_POINT ( 'NONE',  ( 19.99999999999999645, -64.80702306891090814, -7.581672767547114944 ) ) ;
#12503 = EDGE_CURVE ( 'NONE', #15865, #11773, #6777, .T. ) ;
#12504 = CARTESIAN_POINT ( 'NONE',  ( 2.943691928843430450, 14.79893867722910095, 17.48548933151908358 ) ) ;
#12505 = DIRECTION ( 'NONE',  ( -1.000000000000000000, -0.000000000000000000, -0.000000000000000000 ) ) ;
#12506 = EDGE_LOOP ( 'NONE', ( #19773, #3846, #5128, #3808 ) ) ;
#12507 = DIRECTION ( 'NONE',  ( 1.000000000000000000, 0.000000000000000000, 0.000000000000000000 ) ) ;
#12508 = CARTESIAN_POINT ( 'NONE',  ( 17.99999999956958163, -3.580422614997676334, -14.09691874981968773 ) ) ;
#12509 = CARTESIAN_POINT ( 'NONE',  ( 9.999999999999998224, 38.22257254261821657, -61.01667762370101400 ) ) ;
#12510 =( BOUNDED_CURVE ( )  B_SPLINE_CURVE ( 2, ( #4862, #13028, #12830, #11334, #9831, #1788, #19273, #17698, #19483, #8050, #1596, #4968, #14522, #6439, #5058, #12925, #17906 ),
 .UNSPECIFIED., .F., .F. ) 
 B_SPLINE_CURVE_WITH_KNOTS ( ( 3, 2, 2, 2, 2, 2, 2, 2, 3 ),
 ( 0.000000000000000000, 0.01250000000048139860, 0.02500000000096279720, 0.03750000000144419060, 0.05000000000192559441, 0.06250000000240699127, 0.07500000000288838120, 0.08750000000336977113, 0.1000000000038511888 ),
 .UNSPECIFIED. ) 
 CURVE ( )  GEOMETRIC_REPRESENTATION_ITEM ( )  RATIONAL_B_SPLINE_CURVE ( ( 1.000000000000000000, 0.9807852804032304306, 1.000000000000000000, 0.9807852804032304306, 1.000000000000000000, 0.9807852804032304306, 1.000000000000000000, 0.9807852804032304306, 1.000000000000000000, 0.9807852804032304306, 1.000000000000000000, 0.9807852804032304306, 1.000000000000000000, 0.9807852804032304306, 1.000000000000000000, 0.9807852803973104994, 1.000000000005919931 ) ) 
 REPRESENTATION_ITEM ( '' )  );
#12511 = ORIENTED_EDGE ( 'NONE', *, *, #17325, .T. ) ;
#12512 = DIRECTION ( 'NONE',  ( 0.000000000000000000, -0.8878852184023701133, -0.4600650377311617523 ) ) ;
#12513 = ORIENTED_EDGE ( 'NONE', *, *, #3660, .F. ) ;
#12514 = CARTESIAN_POINT ( 'NONE',  ( 36.05404575234035747, -22.88198422515676356, -75.41713818884518616 ) ) ;
#12515 = DIRECTION ( 'NONE',  ( -1.000000000000000000, -0.000000000000000000, -0.000000000000000000 ) ) ;
#12516 = VERTEX_POINT ( 'NONE', #16327 ) ;
#12517 = EDGE_LOOP ( 'NONE', ( #13678, #18176, #191, #10465 ) ) ;
#12518 = CARTESIAN_POINT ( 'NONE',  ( 30.00000000000000000, -105.0000000000000000, -72.35596062816881613 ) ) ;
#12519 = ADVANCED_FACE ( 'NONE', ( #16427 ), #9668, .T. ) ;
#12520 = APPLICATION_CONTEXT ( 'automotive_design' ) ;
#12521 = DIRECTION ( 'NONE',  ( 1.000000000000000000, 0.000000000000000000, 0.000000000000000000 ) ) ;
#12522 = DIRECTION ( 'NONE',  ( -1.000000000000000000, 0.000000000000000000, 0.000000000000000000 ) ) ;
#12523 = DIRECTION ( 'NONE',  ( 1.000000000000000000, 0.000000000000000000, 0.000000000000000000 ) ) ;
#12524 = CARTESIAN_POINT ( 'NONE',  ( -7.500000000000000888, 9.015942588607330751E-10, -23.18869999981969343 ) ) ;
#12525 = PRESENTATION_STYLE_ASSIGNMENT (( #981 ) ) ;
#12526 = DIRECTION ( 'NONE',  ( 0.000000000000000000, 0.000000000000000000, 1.000000000000000000 ) ) ;
#12527 = CARTESIAN_POINT ( 'NONE',  ( -6.165580000000000283, 0.000000000000000000, 7.567219999999999835 ) ) ;
#12528 = ORIENTED_EDGE ( 'NONE', *, *, #6761, .T. ) ;
#12529 = DIRECTION ( 'NONE',  ( 0.000000000000000000, 0.000000000000000000, -1.000000000000000000 ) ) ;
#12530 = VERTEX_POINT ( 'NONE', #3199 ) ;
#12531 = CARTESIAN_POINT ( 'NONE',  ( 12.72792206288790950, 12.72792205982780089, -8.049174999819687315 ) ) ;
#12532 = CARTESIAN_POINT ( 'NONE',  ( 9.999999999999998224, 70.68211945903209426, -13.71269443944134281 ) ) ;
#12533 = ORIENTED_EDGE ( 'NONE', *, *, #18675, .T. ) ;
#12534 = CARTESIAN_POINT ( 'NONE',  ( -10.00000000000000000, 0.000000000000000000, 0.000000000000000000 ) ) ;
#12535 = VERTEX_POINT ( 'NONE', #18025 ) ;
#12536 = FACE_BOUND ( 'NONE', #14423, .T. ) ;
#12537 = DIRECTION ( 'NONE',  ( -1.000000000000000000, 0.000000000000000000, -0.000000000000000000 ) ) ;
#12538 = DIRECTION ( 'NONE',  ( 0.000000000000000000, 0.000000000000000000, -1.000000000000000000 ) ) ;
#12539 = CIRCLE ( 'NONE', #17289, 8.500000000000000000 ) ;
#12540 = ORIENTED_EDGE ( 'NONE', *, *, #17155, .T. ) ;
#12541 = CARTESIAN_POINT ( 'NONE',  ( 19.99999999999999645, -56.63599015375651646, -31.56633360682521072 ) ) ;
#12542 = EDGE_CURVE ( 'NONE', #5755, #12500, #5191, .T. ) ;
#12543 = FACE_OUTER_BOUND ( 'NONE', #10117, .T. ) ;
#12544 = DIRECTION ( 'NONE',  ( 0.000000000000000000, -0.000000000000000000, 1.000000000000000000 ) ) ;
#12545 = FACE_OUTER_BOUND ( 'NONE', #1426, .T. ) ;
#12546 = CIRCLE ( 'NONE', #20658, 65.24900000006526568 ) ;
#12547 = CARTESIAN_POINT ( 'NONE',  ( 52.00000000000000000, -99.99999999999998579, 0.000000000000000000 ) ) ;
#12548 = ORIENTED_EDGE ( 'NONE', *, *, #6048, .T. ) ;
#12549 = DIRECTION ( 'NONE',  ( -1.000000000000000000, -0.000000000000000000, -0.000000000000000000 ) ) ;
#12550 = LINE ( 'NONE', #17110, #11514 ) ;
#12551 = VECTOR ( 'NONE', #6602, 1000.000000000000000 ) ;
#12552 = ORIENTED_EDGE ( 'NONE', *, *, #16188, .T. ) ;
#12553 = LINE ( 'NONE', #19017, #4184 ) ;
#12554 = LINE ( 'NONE', #4708, #3484 ) ;
#12555 = ORIENTED_EDGE ( 'NONE', *, *, #1853, .F. ) ;
#12556 = CARTESIAN_POINT ( 'NONE',  ( -18.00000000043041126, -3.580422610670022099, -9.973481249819688088 ) ) ;
#12557 = CARTESIAN_POINT ( 'NONE',  ( 0.000000000000000000, 19.38316218894295417, -61.87375713200968619 ) ) ;
#12558 = CARTESIAN_POINT ( 'NONE',  ( 2.000000000000027089, 3.464101615137739731, 0.000000000000000000 ) ) ;
#12559 = VERTEX_POINT ( 'NONE', #14848 ) ;
#12560 = CARTESIAN_POINT ( 'NONE',  ( 30.43430782549248903, -42.57363661491096707, -66.38288848018790134 ) ) ;
#12561 = VERTEX_POINT ( 'NONE', #11248 ) ;
#12562 = CARTESIAN_POINT ( 'NONE',  ( 19.99999999999999645, -55.05624179292004072, 35.01774179823764399 ) ) ;
#12563 = TOROIDAL_SURFACE ( 'NONE', #16593, 10.79377999999999993, 0.06721999999999934972 ) ;
#12564 = VERTEX_POINT ( 'NONE', #323 ) ;
#12565 = AXIS2_PLACEMENT_3D ( 'NONE', #12622, #9120, #4240 ) ;
#12566 = CARTESIAN_POINT ( 'NONE',  ( 30.00000000000000000, -106.8560220274159178, 72.71043371383413501 ) ) ;
#12567 = B_SPLINE_CURVE_WITH_KNOTS ( 'NONE', 3,
 ( #4507, #17451, #19032, #12684, #15528, #18933 ),
 .UNSPECIFIED., .F., .F.,
 ( 4, 2, 4 ),
 ( 0.004120275011746849653, 0.005288420935197133549, 0.006456566858647417445 ),
 .UNSPECIFIED. ) ;
#12568 = CARTESIAN_POINT ( 'NONE',  ( 0.2500000000000002220, 0.000000000000000000, 0.000000000000000000 ) ) ;
#12569 = CARTESIAN_POINT ( 'NONE',  ( 2.943691925285398803, -14.79893867793684059, -10.47298933115845188 ) ) ;
#12570 = EDGE_CURVE ( 'NONE', #14189, #17002, #19609, .T. ) ;
#12571 = ORIENTED_EDGE ( 'NONE', *, *, #13639, .T. ) ;
#12572 = EDGE_CURVE ( 'NONE', #18871, #15500, #15724, .T. ) ;
#12573 = CARTESIAN_POINT ( 'NONE',  ( 0.000000000000000000, -64.80702306891090814, -7.581672767547114944 ) ) ;
#12574 = ORIENTED_EDGE ( 'NONE', *, *, #16116, .T. ) ;
#12575 = CARTESIAN_POINT ( 'NONE',  ( 20.81358546886585970, -5.482701416275067352, 87.82403804495045563 ) ) ;
#12576 = VECTOR ( 'NONE', #40, 1000.000000000000000 ) ;
#12577 = CARTESIAN_POINT ( 'NONE',  ( -10.19618095414378445, -15.25966316918061239, 5.793793750180309843 ) ) ;
#12578 = DIRECTION ( 'NONE',  ( 1.000000000000000000, 0.000000000000000000, 0.000000000000000000 ) ) ;
#12579 = TOROIDAL_SURFACE ( 'NONE', #15946, 7.567219999999999835, 0.06721999999999977993 ) ;
#12580 = CARTESIAN_POINT ( 'NONE',  ( 9.999999999999998224, 20.34307325858785731, 69.06634035770315450 ) ) ;
#12581 = EDGE_CURVE ( 'NONE', #11004, #3302, #12694, .T. ) ;
#12582 = ORIENTED_EDGE ( 'NONE', *, *, #3284, .T. ) ;
#12583 = DIRECTION ( 'NONE',  ( -0.000000000000000000, -0.000000000000000000, -1.000000000000000000 ) ) ;
#12584 = CARTESIAN_POINT ( 'NONE',  ( 9.999999999999998224, -53.26727847779572045, 48.44168704307611506 ) ) ;
#12585 = VERTEX_POINT ( 'NONE', #1627 ) ;
#12586 = CARTESIAN_POINT ( 'NONE',  ( -15.15258959384416393, -17.31827655254226528, -78.22681860575444546 ) ) ;
#12587 = CARTESIAN_POINT ( 'NONE',  ( 40.00000000000000711, -122.3205080756887781, -90.00000000000001421 ) ) ;
#12588 = CARTESIAN_POINT ( 'NONE',  ( -2.163827323447877821E-09, -17.99999999999999645, -13.93979999981969442 ) ) ;
#12589 = ORIENTED_EDGE ( 'NONE', *, *, #11168, .F. ) ;
#12590 = CARTESIAN_POINT ( 'NONE',  ( -6.929096494179684207, -2.870125741905212635, -8.087862499819687301 ) ) ;
#12591 = AXIS2_PLACEMENT_3D ( 'NONE', #3121, #12884, #1442 ) ;
#12592 = ADVANCED_FACE ( 'NONE', ( #9553 ), #11552, .F. ) ;
#12593 = CIRCLE ( 'NONE', #5813, 2.649999999999999467 ) ;
#12594 = DIRECTION ( 'NONE',  ( -1.000000000000000000, 0.000000000000000000, 0.000000000000000000 ) ) ;
#12595 = CARTESIAN_POINT ( 'NONE',  ( -52.00000000000000000, -39.99999999999999289, 5.000000000000000000 ) ) ;
#12596 = CARTESIAN_POINT ( 'NONE',  ( 0.000000000000000000, 0.000000000000000000, -130.0000000000000000 ) ) ;
#12597 = AXIS2_PLACEMENT_3D ( 'NONE', #14726, #17810, #6755 ) ;
#12598 = DIRECTION ( 'NONE',  ( -0.7935941825507226710, 0.6084474286424838008, 1.131240564625405124E-16 ) ) ;
#12599 = CARTESIAN_POINT ( 'NONE',  ( 17.99999999956958519, -3.580422614997676778, 4.753081250180309247 ) ) ;
#12600 = EDGE_CURVE ( 'NONE', #14667, #18686, #14548, .T. ) ;
#12601 = EDGE_CURVE ( 'NONE', #349, #12828, #6574, .T. ) ;
#12602 = FACE_OUTER_BOUND ( 'NONE', #2283, .T. ) ;
#12603 = VERTEX_POINT ( 'NONE', #7972 ) ;
#12604 = AXIS2_PLACEMENT_3D ( 'NONE', #2730, #10893, #17367 ) ;
#12605 = DIRECTION ( 'NONE',  ( 0.000000000000000000, 0.000000000000000000, -1.000000000000000000 ) ) ;
#12606 = CARTESIAN_POINT ( 'NONE',  ( 14.79893867758296544, -1.779016607511491977E-09, 19.54720808151908074 ) ) ;
#12607 = EDGE_CURVE ( 'NONE', #13795, #8249, #17726, .T. ) ;
#12608 = FACE_OUTER_BOUND ( 'NONE', #13568, .T. ) ;
#12609 = EDGE_CURVE ( 'NONE', #10422, #20655, #15382, .T. ) ;
#12610 = VECTOR ( 'NONE', #12711, 1000.000000000000000 ) ;
#12611 = VECTOR ( 'NONE', #16533, 1000.000000000000000 ) ;
#12612 = ORIENTED_EDGE ( 'NONE', *, *, #1872, .T. ) ;
#12613 = CIRCLE ( 'NONE', #6171, 75.00000000000000000 ) ;
#12614 = DIRECTION ( 'NONE',  ( 0.000000000000000000, 0.000000000000000000, 1.000000000000000000 ) ) ;
#12615 = DIRECTION ( 'NONE',  ( -0.000000000000000000, -0.000000000000000000, -1.000000000000000000 ) ) ;
#12616 = CARTESIAN_POINT ( 'NONE',  ( 30.43430782549247837, -42.57363661491096707, -71.38288848018790134 ) ) ;
#12617 = AXIS2_PLACEMENT_3D ( 'NONE', #11126, #4971, #93 ) ;
#12618 = ORIENTED_EDGE ( 'NONE', *, *, #14250, .T. ) ;
#12619 = DIRECTION ( 'NONE',  ( -0.000000000000000000, -0.000000000000000000, 1.000000000000000000 ) ) ;
#12620 = ORIENTED_EDGE ( 'NONE', *, *, #14658, .F. ) ;
#12621 = ADVANCED_FACE ( 'NONE', ( #19405 ), #4893, .T. ) ;
#12622 = CARTESIAN_POINT ( 'NONE',  ( 6.679999999999998828, 7.059243326609123303E-15, 0.000000000000000000 ) ) ;
#12623 = CARTESIAN_POINT ( 'NONE',  ( 9.999999999999998224, 71.76067541710858677, -5.865617076723870227 ) ) ;
#12624 = ORIENTED_EDGE ( 'NONE', *, *, #6397, .F. ) ;
#12625 = EDGE_CURVE ( 'NONE', #18498, #7039, #16393, .T. ) ;
#12626 = VERTEX_POINT ( 'NONE', #9766 ) ;
#12627 = CARTESIAN_POINT ( 'NONE',  ( 31.94823399543905040, -113.6545208995224954, -75.04431888125806438 ) ) ;
#12628 = ADVANCED_FACE ( 'NONE', ( #16231 ), #8167, .T. ) ;
#12629 = EDGE_CURVE ( 'NONE', #16541, #19870, #5232, .T. ) ;
#12630 =( NAMED_UNIT ( * ) SI_UNIT ( $, .STERADIAN. ) SOLID_ANGLE_UNIT ( ) );
#12631 = CARTESIAN_POINT ( 'NONE',  ( 19.99999999999999645, -24.01204443665145405, -60.22865198596149838 ) ) ;
#12632 = CIRCLE ( 'NONE', #9574, 2.041999999999999815 ) ;
#12633 = VECTOR ( 'NONE', #19137, 1000.000000000000000 ) ;
#12634 = EDGE_CURVE ( 'NONE', #10983, #16643, #2862, .T. ) ;
#12635 = CARTESIAN_POINT ( 'NONE',  ( 6.250000000000054179, 10.82531754730546147, 166.0000000000000000 ) ) ;
#12637 = AXIS2_PLACEMENT_3D ( 'NONE', #16189, #6421, #8122 ) ;
#12636 = CARTESIAN_POINT ( 'NONE',  ( 4.276731815070943910, 10.32494394706616703, -13.54957774935257753 ) ) ;
#12638 = CARTESIAN_POINT ( 'NONE',  ( 5.303300858261582817, -5.303300859536631329, -26.72307499981969059 ) ) ;
#12639 = CARTESIAN_POINT ( 'NONE',  ( -2.000000000000009770, 3.464101615137749057, 0.000000000000000000 ) ) ;
#12640 = AXIS2_PLACEMENT_3D ( 'NONE', #19343, #3340, #6313 ) ;
#12641 = CARTESIAN_POINT ( 'NONE',  ( 0.000000000000000000, 53.26727847779537939, 48.44168704307649875 ) ) ;
#12642 = CARTESIAN_POINT ( 'NONE',  ( 19.99999999999999645, 38.22257254261739945, 61.01667762370151138 ) ) ;
#12643 = VERTEX_POINT ( 'NONE', #20012 ) ;
#12644 = DIRECTION ( 'NONE',  ( 0.000000000000000000, 0.000000000000000000, 1.000000000000000000 ) ) ;
#12645 = ORIENTED_EDGE ( 'NONE', *, *, #4009, .F. ) ;
#12646 = CARTESIAN_POINT ( 'NONE',  ( -16.62983158603122291, -6.888301780572501087, -21.59761249981969300 ) ) ;
#12647 = CARTESIAN_POINT ( 'NONE',  ( 19.99999999999999645, -11.98658579560631843, 64.13855129306463709 ) ) ;
#12648 = VECTOR ( 'NONE', #7585, 1000.000000000000000 ) ;
#12649 = EDGE_LOOP ( 'NONE', ( #2207, #4323, #9554, #15342 ) ) ;
#12650 = VECTOR ( 'NONE', #2044, 1000.000000000000000 ) ;
#12651 = DIRECTION ( 'NONE',  ( -1.000000000000000000, 0.000000000000000000, 0.000000000000000000 ) ) ;
#12652 = VERTEX_POINT ( 'NONE', #5298 ) ;
#12653 = CARTESIAN_POINT ( 'NONE',  ( -9.015947181032828388E-10, -7.500000000000002665, -6.694949999819694852 ) ) ;
#12654 = CARTESIAN_POINT ( 'NONE',  ( 4.925000000000044231, 8.530350227276702668, -43.00000000000000000 ) ) ;
#12655 = CARTESIAN_POINT ( 'NONE',  ( -7.500000000000000000, 0.000000000000000000, 40.00000000000000000 ) ) ;
#12656 = ORIENTED_EDGE ( 'NONE', *, *, #4019, .F. ) ;
#12657 = LINE ( 'NONE', #10843, #12034 ) ;
#12658 = AXIS2_PLACEMENT_3D ( 'NONE', #5979, #6077, #19231 ) ;
#12659 = DIRECTION ( 'NONE',  ( 0.000000000000000000, 0.000000000000000000, 1.000000000000000000 ) ) ;
#12660 = DIRECTION ( 'NONE',  ( -0.000000000000000000, -0.000000000000000000, -1.000000000000000000 ) ) ;
#12661 = DIRECTION ( 'NONE',  ( -0.000000000000000000, -0.000000000000000000, -1.000000000000000000 ) ) ;
#12662 = AXIS2_PLACEMENT_3D ( 'NONE', #2980, #20664, #6146 ) ;
#12663 = DIRECTION ( 'NONE',  ( 0.000000000000000000, 0.000000000000000000, 1.000000000000000000 ) ) ;
#12664 = ORIENTED_EDGE ( 'NONE', *, *, #9379, .F. ) ;
#12665 = CARTESIAN_POINT ( 'NONE',  ( -2.000000000000009770, 3.464101615137749057, 0.000000000000000000 ) ) ;
#12666 = CARTESIAN_POINT ( 'NONE',  ( -7.500000000000009770, 9.706494107251932559E-15, 1.926200000002316060 ) ) ;
#12667 = ORIENTED_EDGE ( 'NONE', *, *, #14140, .T. ) ;
#12668 = DIRECTION ( 'NONE',  ( 0.000000000000000000, -8.673617379884036705E-17, 1.000000000000000000 ) ) ;
#12669 = CARTESIAN_POINT ( 'NONE',  ( -5.303300858261589035, 5.303300859536635770, -6.320674999819683393 ) ) ;
#12670 = ADVANCED_FACE ( 'NONE', ( #16535 ), #8581, .F. ) ;
#12671 = ORIENTED_EDGE ( 'NONE', *, *, #15716, .T. ) ;
#12672 = EDGE_CURVE ( 'NONE', #13929, #5677, #19122, .T. ) ;
#12673 = CARTESIAN_POINT ( 'NONE',  ( -17.99999999956958519, 3.580422614997674113, -9.384418749819685601 ) ) ;
#12674 = DIRECTION ( 'NONE',  ( 1.000000000000000000, 1.836909530733573776E-16, 0.000000000000000000 ) ) ;
#12675 = DIRECTION ( 'NONE',  ( -1.000000000000000000, 0.000000000000000000, 0.000000000000000000 ) ) ;
#12676 = CIRCLE ( 'NONE', #3503, 2.649999999999999467 ) ;
#12677 = ORIENTED_EDGE ( 'NONE', *, *, #18143, .T. ) ;
#12678 = CIRCLE ( 'NONE', #3175, 4.250000000000000000 ) ;
#12679 = CARTESIAN_POINT ( 'NONE',  ( 19.99999999999999645, 0.000000000000000000, 0.000000000000000000 ) ) ;
#12680 = ORIENTED_EDGE ( 'NONE', *, *, #8441, .F. ) ;
#12681 = DIRECTION ( 'NONE',  ( 1.000000000000000000, 0.000000000000000000, 0.000000000000000000 ) ) ;
#12682 = ORIENTED_EDGE ( 'NONE', *, *, #3910, .F. ) ;
#12683 = AXIS2_PLACEMENT_3D ( 'NONE', #12880, #14669, #19632 ) ;
#12684 = CARTESIAN_POINT ( 'NONE',  ( 4.000000000000003553, -0.7779732554280840429, -5.566455648918319454 ) ) ;
#12685 = CARTESIAN_POINT ( 'NONE',  ( 0.000000000000000000, 6.872116855663142232, 64.47358224882421496 ) ) ;
#12686 = AXIS2_PLACEMENT_3D ( 'NONE', #1218, #1326, #5967 ) ;
#12687 = ADVANCED_FACE ( 'NONE', ( #14951 ), #3907, .T. ) ;
#12688 = CARTESIAN_POINT ( 'NONE',  ( -9.474249097082500626, 6.330490858644140850, 22.08870350064742993 ) ) ;
#12689 = ORIENTED_EDGE ( 'NONE', *, *, #3140, .F. ) ;
#12690 = CARTESIAN_POINT ( 'NONE',  ( -9.015947181032828388E-10, -7.500000000000002665, -16.11994999981969556 ) ) ;
#12691 = CARTESIAN_POINT ( 'NONE',  ( -30.00000000000000000, -151.4095880458873467, -44.60680010464253087 ) ) ;
#12692 = ORIENTED_EDGE ( 'NONE', *, *, #296, .F. ) ;
#12693 = CARTESIAN_POINT ( 'NONE',  ( 2.822967073032372820, -21.36251226604836617, 76.10389727344437460 ) ) ;
#12694 = CIRCLE ( 'NONE', #7949, 10.00000000000000178 ) ;
#12695 = EDGE_CURVE ( 'NONE', #12251, #9297, #8957, .T. ) ;
#12696 = CARTESIAN_POINT ( 'NONE',  ( 7.500000000000004441, 1.491842754878798027, -18.77073124991221320 ) ) ;
#12697 = DIRECTION ( 'NONE',  ( -0.000000000000000000, 0.7812527682501551052, 0.6242147964454779485 ) ) ;
#12698 = ORIENTED_EDGE ( 'NONE', *, *, #6098, .T. ) ;
#12699 = DIRECTION ( 'NONE',  ( 0.000000000000000000, 0.000000000000000000, -1.000000000000000000 ) ) ;
#12700 = FACE_OUTER_BOUND ( 'NONE', #8514, .T. ) ;
#12701 =( GEOMETRIC_REPRESENTATION_CONTEXT ( 3 ) GLOBAL_UNCERTAINTY_ASSIGNED_CONTEXT ( ( #7291 ) ) GLOBAL_UNIT_ASSIGNED_CONTEXT ( ( #16732, #15462, #7395 ) ) REPRESENTATION_CONTEXT ( 'NONE', 'WORKASPACE' ) );
#12702 = ORIENTED_EDGE ( 'NONE', *, *, #8624, .F. ) ;
#12703 = EDGE_CURVE ( 'NONE', #12774, #17279, #11770, .T. ) ;
#12704 = CARTESIAN_POINT ( 'NONE',  ( -6.999999999999995559, 4.546351088565595293E-15, 0.000000000000000000 ) ) ;
#12705 = DIRECTION ( 'NONE',  ( 0.000000000000000000, 0.000000000000000000, -1.000000000000000000 ) ) ;
#12706 = CARTESIAN_POINT ( 'NONE',  ( 10.19618095047497697, -15.25966317163202923, -14.82339374981969016 ) ) ;
#12707 = ORIENTED_EDGE ( 'NONE', *, *, #20199, .F. ) ;
#12708 = CARTESIAN_POINT ( 'NONE',  ( -10.00000000000000000, 0.000000000000000000, 0.000000000000000000 ) ) ;
#12709 = CIRCLE ( 'NONE', #1550, 205.0000000000000284 ) ;
#12710 = DIRECTION ( 'NONE',  ( 0.000000000000000000, 0.000000000000000000, 1.000000000000000000 ) ) ;
#12711 = DIRECTION ( 'NONE',  ( 1.000000000000000000, 0.000000000000000000, -0.000000000000000000 ) ) ;
#12712 = ADVANCED_FACE ( 'NONE', ( #13368 ), #13676, .F. ) ;
#12713 = DIRECTION ( 'NONE',  ( 6.982962677686266711E-15, 0.000000000000000000, -1.000000000000000000 ) ) ;
#12714 = CARTESIAN_POINT ( 'NONE',  ( -3.580422614997675890, -17.99999999956958519, -2.315668749819692618 ) ) ;
#12715 = EDGE_CURVE ( 'NONE', #2314, #6220, #13787, .T. ) ;
#12716 = CARTESIAN_POINT ( 'NONE',  ( -6.929096494179684207, -2.870125741905212635, -17.51286249981968979 ) ) ;
#12717 = ORIENTED_EDGE ( 'NONE', *, *, #2084, .T. ) ;
#12718 = LINE ( 'NONE', #12719, #12102 ) ;
#12719 = CARTESIAN_POINT ( 'NONE',  ( 19.99999999999999645, -3.141410481200616278, -65.17333458706190186 ) ) ;
#12720 = CARTESIAN_POINT ( 'NONE',  ( 12.54593441764186679, 8.382925368423272516, 9.238614331519077183 ) ) ;
#12721 = DIRECTION ( 'NONE',  ( 1.000000000000000000, 1.836909530733573776E-16, 0.000000000000000000 ) ) ;
#12722 = VECTOR ( 'NONE', #10850, 1000.000000000000000 ) ;
#12723 = ORIENTED_EDGE ( 'NONE', *, *, #16095, .T. ) ;
#12724 = CARTESIAN_POINT ( 'NONE',  ( 0.000000000000000000, 0.000000000000000000, 0.000000000000000000 ) ) ;
#12725 = FACE_OUTER_BOUND ( 'NONE', #10514, .T. ) ;
#12726 = CARTESIAN_POINT ( 'NONE',  ( 30.02285928914783142, -48.02662919861900548, 66.64486488415462873 ) ) ;
#12727 = VERTEX_POINT ( 'NONE', #16856 ) ;
#12728 = ADVANCED_FACE ( 'NONE', ( #7304 ), #18444, .F. ) ;
#12729 = CARTESIAN_POINT ( 'NONE',  ( 4.000000000000003553, 2.309401076758480720, -5.599999999999999645 ) ) ;
#12730 = EDGE_LOOP ( 'NONE', ( #973, #4211, #11641, #15757 ) ) ;
#12731 = DIRECTION ( 'NONE',  ( -0.000000000000000000, -0.000000000000000000, 1.000000000000000000 ) ) ;
#12732 = DIRECTION ( 'NONE',  ( 0.000000000000000000, -0.8878852184023701133, -0.4600650377311617523 ) ) ;
#12733 = ADVANCED_FACE ( 'NONE', ( #19815 ), #3601, .T. ) ;
#12734 = VERTEX_POINT ( 'NONE', #15255 ) ;
#12735 = ORIENTED_EDGE ( 'NONE', *, *, #2205, .T. ) ;
#12736 = CARTESIAN_POINT ( 'NONE',  ( 18.00000000000000000, -2.163824016901520184E-09, 22.35625000018031372 ) ) ;
#12737 = AXIS2_PLACEMENT_3D ( 'NONE', #4739, #19463, #7921 ) ;
#12738 = EDGE_CURVE ( 'NONE', #9460, #3717, #740, .T. ) ;
#12739 = ADVANCED_FACE ( 'NONE', ( #10078, #16948, #2123, #8896, #2019, #15056 ), #429, .T. ) ;
#12740 = CARTESIAN_POINT ( 'NONE',  ( 2.500000000000000000, 0.000000000000000000, 2.041999999999999815 ) ) ;
#12741 = AXIS2_PLACEMENT_3D ( 'NONE', #15908, #17516, #13907 ) ;
#12742 = CARTESIAN_POINT ( 'NONE',  ( 0.000000000000000000, 53.26727847779604019, -48.44168704307576689 ) ) ;
#12743 = CARTESIAN_POINT ( 'NONE',  ( 9.474249097082498849, -6.330490858644140850, -10.89879649935257433 ) ) ;
#12744 = CARTESIAN_POINT ( 'NONE',  ( 5.303300858261582817, -5.303300859536631329, -17.29807499981968988 ) ) ;
#12745 = DIRECTION ( 'NONE',  ( -1.000000000000000000, -0.000000000000000000, -0.000000000000000000 ) ) ;
#12746 = EDGE_CURVE ( 'NONE', #19589, #8077, #20552, .T. ) ;
#12747 = FACE_OUTER_BOUND ( 'NONE', #1558, .T. ) ;
#12748 = DIRECTION ( 'NONE',  ( 1.000000000000000000, 1.836909530733573776E-16, 0.000000000000000000 ) ) ;
#12749 = ADVANCED_FACE ( 'NONE', ( #638 ), #17278, .F. ) ;
#12750 =( GEOMETRIC_REPRESENTATION_CONTEXT ( 3 ) GLOBAL_UNCERTAINTY_ASSIGNED_CONTEXT ( ( #526 ) ) GLOBAL_UNIT_ASSIGNED_CONTEXT ( ( #19696, #12278, #18754 ) ) REPRESENTATION_CONTEXT ( 'NONE', 'WORKASPACE' ) );
#12751 = ORIENTED_EDGE ( 'NONE', *, *, #18678, .T. ) ;
#12752 = CYLINDRICAL_SURFACE ( 'NONE', #17001, 7.500000000000000000 ) ;
#12753 = VECTOR ( 'NONE', #8592, 1000.000000000000000 ) ;
#12754 = ORIENTED_EDGE ( 'NONE', *, *, #9539, .F. ) ;
#12755 = CARTESIAN_POINT ( 'NONE',  ( 12.72792205982779734, -12.72792206288791128, -15.11792499981968696 ) ) ;
#12756 = CARTESIAN_POINT ( 'NONE',  ( 30.00000000000000000, -30.00000000000000711, 44.99999999999998579 ) ) ;
#12757 = EDGE_LOOP ( 'NONE', ( #10837, #5663 ) ) ;
#12758 = CARTESIAN_POINT ( 'NONE',  ( -22.70866746290765903, -3.649167310370807105, -90.00000000000000000 ) ) ;
#12759 = VECTOR ( 'NONE', #20701, 1000.000000000000000 ) ;
#12760 = EDGE_LOOP ( 'NONE', ( #4584, #11022, #6778, #6915 ) ) ;
#12761 = VECTOR ( 'NONE', #1971, 1000.000000000000000 ) ;
#12762 = LINE ( 'NONE', #9356, #6108 ) ;
#12763 = DIRECTION ( 'NONE',  ( 0.000000000000000000, -0.000000000000000000, 1.000000000000000000 ) ) ;
#12764 = CARTESIAN_POINT ( 'NONE',  ( -1.491842754445841690, 7.500000000179340987, -2.276981249819693520 ) ) ;
#12765 = EDGE_CURVE ( 'NONE', #12727, #17488, #6037, .T. ) ;
#12766 = ORIENTED_EDGE ( 'NONE', *, *, #12609, .F. ) ;
#12767 = DIRECTION ( 'NONE',  ( -1.000000000000000000, 0.000000000000000000, 0.000000000000000000 ) ) ;
#12768 = CIRCLE ( 'NONE', #19851, 2.041999999999999815 ) ;
#12769 = CARTESIAN_POINT ( 'NONE',  ( 12.72792205982779379, -12.72792206288790950, -24.54292499981969300 ) ) ;
#12770 = CARTESIAN_POINT ( 'NONE',  ( 0.000000000000000000, 6.872116855664026858, -64.47358224882410127 ) ) ;
#12771 = AXIS2_PLACEMENT_3D ( 'NONE', #4378, #12121, #13924 ) ;
#12772 = AXIS2_PLACEMENT_3D ( 'NONE', #2642, #15974, #19058 ) ;
#12773 = DIRECTION ( 'NONE',  ( -1.000000000000000000, 0.000000000000000000, -0.000000000000000000 ) ) ;
#12774 = VERTEX_POINT ( 'NONE', #7831 ) ;
#12775 = CARTESIAN_POINT ( 'NONE',  ( 9.999999999999998224, -38.22257254261782577, 61.01667762370126269 ) ) ;
#12776 = PRESENTATION_LAYER_ASSIGNMENT (  '', '', ( #1642 ) ) ;
#12777 = DIRECTION ( 'NONE',  ( -0.8660254037844372643, -0.5000000000000024425, 0.000000000000000000 ) ) ;
#12778 = ORIENTED_EDGE ( 'NONE', *, *, #554, .T. ) ;
#12779 = DIRECTION ( 'NONE',  ( -1.000000000000000000, -0.000000000000000000, -0.000000000000000000 ) ) ;
#12780 = DIRECTION ( 'NONE',  ( 0.000000000000000000, 0.000000000000000000, -1.000000000000000000 ) ) ;
#12781 = EDGE_CURVE ( 'NONE', #12057, #17356, #5307, .T. ) ;
#12782 = VERTEX_POINT ( 'NONE', #10909 ) ;
#12783 = DIRECTION ( 'NONE',  ( -0.000000000000000000, -0.000000000000000000, -1.000000000000000000 ) ) ;
#12784 = CARTESIAN_POINT ( 'NONE',  ( 21.50000000000000000, 2.632990618166809235E-15, -68.00000000000000000 ) ) ;
#12785 = DIRECTION ( 'NONE',  ( 1.000000000000000000, 0.000000000000000000, 0.000000000000000000 ) ) ;
#12786 = AXIS2_PLACEMENT_3D ( 'NONE', #2549, #14105, #20558 ) ;
#12787 = ORIENTED_EDGE ( 'NONE', *, *, #8367, .F. ) ;
#12788 = CARTESIAN_POINT ( 'NONE',  ( -30.00000000000000000, 36.35083268962915781, -50.00000000000000000 ) ) ;
#12789 = EDGE_LOOP ( 'NONE', ( #823, #6157 ) ) ;
#12790 = CARTESIAN_POINT ( 'NONE',  ( -52.49999999999999289, -120.0000000000000142, 5.000000000000000000 ) ) ;
#12791 = AXIS2_PLACEMENT_3D ( 'NONE', #17983, #9817, #5143 ) ;
#12792 = ORIENTED_EDGE ( 'NONE', *, *, #6389, .F. ) ;
#12793 = VECTOR ( 'NONE', #9716, 1000.000000000000000 ) ;
#12794 = CONICAL_SURFACE ( 'NONE', #19530, 2.055000000000000160, 0.7853981633974639331 ) ;
#12795 = CARTESIAN_POINT ( 'NONE',  ( 0.000000000000000000, -45.48683723007179935, -46.78012013466265984 ) ) ;
#12796 = EDGE_CURVE ( 'NONE', #11637, #19132, #7699, .T. ) ;
#12797 = DIRECTION ( 'NONE',  ( -1.000000000000000000, 0.000000000000000000, 0.000000000000000000 ) ) ;
#12798 = CARTESIAN_POINT ( 'NONE',  ( 2.222972768810839383, -11.17563879758428769, 18.55432850064742922 ) ) ;
#12799 = VERTEX_POINT ( 'NONE', #20331 ) ;
#12800 = CARTESIAN_POINT ( 'NONE',  ( 0.000000000000000000, -59.31169354540720207, -27.19476070466916795 ) ) ;
#12801 = AXIS2_PLACEMENT_3D ( 'NONE', #2922, #17129, #12246 ) ;
#12802 = CARTESIAN_POINT ( 'NONE',  ( 30.00000000000000000, -110.0000000000000000, -45.00000000000000711 ) ) ;
#12803 = ORIENTED_EDGE ( 'NONE', *, *, #16929, .F. ) ;
#12804 = LINE ( 'NONE', #14071, #15222 ) ;
#12805 = VECTOR ( 'NONE', #19214, 1000.000000000000000 ) ;
#12806 = CYLINDRICAL_SURFACE ( 'NONE', #19333, 72.00000000007199219 ) ;
#12807 = DIRECTION ( 'NONE',  ( 1.000000000000000000, -0.000000000000000000, -0.000000000000000000 ) ) ;
#12808 = VERTEX_POINT ( 'NONE', #9433 ) ;
#12809 = CARTESIAN_POINT ( 'NONE',  ( 19.99999999999999645, 18.50424539729845463, 69.58155576219121485 ) ) ;
#12810 = DIRECTION ( 'NONE',  ( -1.000000000000000000, -0.000000000000000000, -0.000000000000000000 ) ) ;
#12811 =( REPRESENTATION_RELATIONSHIP ('NONE','NONE', #13739, #11016 ) REPRESENTATION_RELATIONSHIP_WITH_TRANSFORMATION ( #19886 )SHAPE_REPRESENTATION_RELATIONSHIP( ) );
#12812 = ORIENTED_EDGE ( 'NONE', *, *, #12360, .F. ) ;
#12813 = CARTESIAN_POINT ( 'NONE',  ( -18.07215471859532485, -14.28798666575421628, -80.13107141598003125 ) ) ;
#12814 = DIRECTION ( 'NONE',  ( -0.000000000000000000, -0.000000000000000000, -1.000000000000000000 ) ) ;
#12815 = CARTESIAN_POINT ( 'NONE',  ( 19.99999999999999645, 36.54710069451126486, -54.05313526368077248 ) ) ;
#12816 = ORIENTED_EDGE ( 'NONE', *, *, #13328, .T. ) ;
#12817 = CARTESIAN_POINT ( 'NONE',  ( 43.62500077266424370, -124.9999999999999858, -90.00000000000001421 ) ) ;
#12818 = CYLINDRICAL_SURFACE ( 'NONE', #13948, 65.24900000006525147 ) ;
#12819 = EDGE_CURVE ( 'NONE', #19326, #14998, #10747, .T. ) ;
#12820 = CARTESIAN_POINT ( 'NONE',  ( 19.99999999999999645, -6.872116855662673274, -64.47358224882424338 ) ) ;
#12821 = CARTESIAN_POINT ( 'NONE',  ( 6.249999999999902300, -10.82531754730554496, 51.00000000000001421 ) ) ;
#12822 = CARTESIAN_POINT ( 'NONE',  ( 10.19618095414378978, 15.25966316918061771, -6.439106249819692707 ) ) ;
#12823 = DIRECTION ( 'NONE',  ( -1.000000000000000000, -0.000000000000000000, -0.000000000000000000 ) ) ;
#12824 = FACE_OUTER_BOUND ( 'NONE', #12730, .T. ) ;
#12825 = EDGE_CURVE ( 'NONE', #18745, #19852, #13116, .T. ) ;
#12826 = CARTESIAN_POINT ( 'NONE',  ( -14.79893867758296544, 1.779018419858780125E-09, -4.015291918480927258 ) ) ;
#12827 = CARTESIAN_POINT ( 'NONE',  ( 42.61160110135222823, -124.0569253416645523, -88.80170281571382418 ) ) ;
#12828 = VERTEX_POINT ( 'NONE', #15889 ) ;
#12829 = FACE_OUTER_BOUND ( 'NONE', #16260, .T. ) ;
#12830 = CARTESIAN_POINT ( 'NONE',  ( 6.929096494179683319, 2.870125741905213079, 24.89963750018031519 ) ) ;
#12831 = CARTESIAN_POINT ( 'NONE',  ( 36.91783118030027566, -21.11288316874070858, 70.73473707049505776 ) ) ;
#12832 = ORIENTED_EDGE ( 'NONE', *, *, #11183, .T. ) ;
#12833 = LINE ( 'NONE', #6442, #14967 ) ;
#12834 = ORIENTED_EDGE ( 'NONE', *, *, #20084, .F. ) ;
#12835 = DIRECTION ( 'NONE',  ( 0.000000000000000000, 0.000000000000000000, 1.000000000000000000 ) ) ;
#12836 = CARTESIAN_POINT ( 'NONE',  ( 15.25966317163202568, 10.19618095047498230, 20.52035625018030984 ) ) ;
#12837 = ORIENTED_EDGE ( 'NONE', *, *, #8925, .F. ) ;
#12838 = ORIENTED_EDGE ( 'NONE', *, *, #1328, .F. ) ;
#12839 = LINE ( 'NONE', #4355, #2243 ) ;
#12840 = SHAPE_REPRESENTATION_RELATIONSHIP ( 'NONE' , 'NONE' ,  #7225, #11209 ) ;
#12841 = CARTESIAN_POINT ( 'NONE',  ( 0.000000000000000000, 0.000000000000000000, -90.00000000000000000 ) ) ;
#12842 = CARTESIAN_POINT ( 'NONE',  ( 1.040949779275250179E-14, -85.00000000000000000, 5.000000000000000000 ) ) ;
#12843 = CARTESIAN_POINT ( 'NONE',  ( 4.276731815070943910, 10.32494394706616703, -4.124577749352575040 ) ) ;
#12844 = EDGE_CURVE ( 'NONE', #281, #8899, #20652, .T. ) ;
#12845 = CARTESIAN_POINT ( 'NONE',  ( 6.330490858644138186, 9.474249097082495297, 17.32223399971320532 ) ) ;
#12846 = EDGE_CURVE ( 'NONE', #13708, #3116, #17384, .T. ) ;
#12847 = CARTESIAN_POINT ( 'NONE',  ( 19.99999999999999645, -8.857208570069305509, -71.45313048675095047 ) ) ;
#12848 = FACE_BOUND ( 'NONE', #2257, .T. ) ;
#12849 = DIRECTION ( 'NONE',  ( 0.000000000000000000, 0.000000000000000000, -1.000000000000000000 ) ) ;
#12850 = ORIENTED_EDGE ( 'NONE', *, *, #16399, .F. ) ;
#12851 = DIRECTION ( 'NONE',  ( 0.000000000000000000, 0.000000000000000000, 1.000000000000000000 ) ) ;
#12852 = ORIENTED_EDGE ( 'NONE', *, *, #13134, .T. ) ;
#12853 = CARTESIAN_POINT ( 'NONE',  ( -16.62983158437510056, 6.888301784570729502, 9.760112500180312622 ) ) ;
#12854 = CARTESIAN_POINT ( 'NONE',  ( 0.000000000000000000, 63.85430960833490843, -11.25592921604860663 ) ) ;
#12855 = EDGE_CURVE ( 'NONE', #2608, #20537, #7619, .T. ) ;
#12856 = ORIENTED_EDGE ( 'NONE', *, *, #1346, .T. ) ;
#12857 = CARTESIAN_POINT ( 'NONE',  ( -10.00000000000000000, 0.000000000000000000, 0.000000000000000000 ) ) ;
#12858 = ORIENTED_EDGE ( 'NONE', *, *, #1459, .F. ) ;
#12859 = CARTESIAN_POINT ( 'NONE',  ( 17.50000000000000355, 0.000000000000000000, 126.0000000000000000 ) ) ;
#12860 = CARTESIAN_POINT ( 'NONE',  ( 31.48871417509230142, -36.16658848463109166, 71.75696761739389729 ) ) ;
#12861 = ORIENTED_EDGE ( 'NONE', *, *, #8793, .F. ) ;
#12862 = DIRECTION ( 'NONE',  ( 1.000000000000000000, 0.000000000000000000, -0.000000000000000000 ) ) ;
#12863 = DIRECTION ( 'NONE',  ( 0.000000000000000000, 0.6310879443260540844, -0.7757112907044187988 ) ) ;
#12864 = CARTESIAN_POINT ( 'NONE',  ( -12.50000000000000533, 0.000000000000000000, 126.0000000000000000 ) ) ;
#12865 = ADVANCED_FACE ( 'NONE', ( #9323 ), #6134, .F. ) ;
#12866 = FACE_BOUND ( 'NONE', #5908, .T. ) ;
#12867 = VERTEX_POINT ( 'NONE', #11015 ) ;
#12868 = EDGE_CURVE ( 'NONE', #15181, #2818, #2857, .T. ) ;
#12869 = AXIS2_PLACEMENT_3D ( 'NONE', #19558, #13201, #14791 ) ;
#12870 = CYLINDRICAL_SURFACE ( 'NONE', #1215, 2.500000000000000444 ) ;
#12871 = EDGE_CURVE ( 'NONE', #3436, #1656, #17861, .T. ) ;
#12872 = CARTESIAN_POINT ( 'NONE',  ( -14.49999999999998934, -85.00000000000000000, 19.00000000000000000 ) ) ;
#12873 = EDGE_LOOP ( 'NONE', ( #6752, #13629, #2120, #7417 ) ) ;
#12874 = DIRECTION ( 'NONE',  ( 0.000000000000000000, 0.9976687691905389288, 0.06824241336467461172 ) ) ;
#12875 = DIRECTION ( 'NONE',  ( -1.000000000000000000, -0.000000000000000000, -0.000000000000000000 ) ) ;
#12876 = ADVANCED_FACE ( 'NONE', ( #10603 ), #13995, .F. ) ;
#12877 = ORIENTED_EDGE ( 'NONE', *, *, #12894, .T. ) ;
#12878 = CARTESIAN_POINT ( 'NONE',  ( 0.000000000000000000, -10.77748419466740692, 63.93680186330469439 ) ) ;
#12879 = DIRECTION ( 'NONE',  ( -1.000000000000000000, 0.000000000000000000, 0.000000000000000000 ) ) ;
#12880 = CARTESIAN_POINT ( 'NONE',  ( 0.000000000000000000, 0.000000000000000000, -81.99999999999998579 ) ) ;
#12881 = ORIENTED_EDGE ( 'NONE', *, *, #18415, .T. ) ;
#12882 = CARTESIAN_POINT ( 'NONE',  ( 0.000000000000000000, -20.34307325858738835, -69.06634035770328239 ) ) ;
#12883 = ORIENTED_EDGE ( 'NONE', *, *, #12420, .T. ) ;
#12884 = DIRECTION ( 'NONE',  ( -0.000000000000000000, -0.000000000000000000, -1.000000000000000000 ) ) ;
#12885 = VERTEX_POINT ( 'NONE', #14208 ) ;
#12886 = DIRECTION ( 'NONE',  ( 0.000000000000000000, 0.000000000000000000, 1.000000000000000000 ) ) ;
#12887 = EDGE_CURVE ( 'NONE', #7047, #4467, #20207, .T. ) ;
#12888 = EDGE_CURVE ( 'NONE', #20602, #14689, #6999, .T. ) ;
#12889 = DIRECTION ( 'NONE',  ( -0.4999999999999918954, 0.8660254037844433705, 0.000000000000000000 ) ) ;
#12890 = VECTOR ( 'NONE', #8105, 1000.000000000000000 ) ;
#12891 = CARTESIAN_POINT ( 'NONE',  ( 10.46442989202484064, -10.46442989454075878, -11.35658308115845472 ) ) ;
#12892 = ORIENTED_EDGE ( 'NONE', *, *, #16469, .F. ) ;
#12893 = CARTESIAN_POINT ( 'NONE',  ( -7.500000000000000000, 0.000000000000000000, -40.00000000000000000 ) ) ;
#12894 = EDGE_CURVE ( 'NONE', #3863, #19670, #3611, .T. ) ;
#12895 = CARTESIAN_POINT ( 'NONE',  ( 50.00000000000000000, -124.9999999999999858, -90.00000000000001421 ) ) ;
#12896 = EDGE_LOOP ( 'NONE', ( #13916, #9468 ) ) ;
#12897 = CARTESIAN_POINT ( 'NONE',  ( -1.491842756249031954, -7.499999999820663454, -25.25041874981969414 ) ) ;
#12898 = CARTESIAN_POINT ( 'NONE',  ( 10.00000000000000178, -160.0000000000000000, -70.00000000000000000 ) ) ;
#12899 = DIRECTION ( 'NONE',  ( 1.000000000000000000, -0.000000000000000000, -0.000000000000000000 ) ) ;
#12900 = CARTESIAN_POINT ( 'NONE',  ( 17.50000000000000355, 0.000000000000000000, 166.0000000000000000 ) ) ;
#12901 = VERTEX_POINT ( 'NONE', #18875 ) ;
#12902 = AXIS2_PLACEMENT_3D ( 'NONE', #7322, #2349, #5625 ) ;
#12903 = EDGE_CURVE ( 'NONE', #12002, #6701, #8370, .T. ) ;
#12904 = LINE ( 'NONE', #14503, #10060 ) ;
#12905 = CIRCLE ( 'NONE', #1395, 27.60000000002759890 ) ;
#12906 = VERTEX_POINT ( 'NONE', #19274 ) ;
#12907 = CARTESIAN_POINT ( 'NONE',  ( 19.99999999999999645, 0.000000000000000000, 0.000000000000000000 ) ) ;
#12908 = CARTESIAN_POINT ( 'NONE',  ( 0.6543461111163461075, 4.241015250120812929, -5.460849780464856806 ) ) ;
#12909 = ORIENTED_EDGE ( 'NONE', *, *, #18694, .F. ) ;
#12910 = DIRECTION ( 'NONE',  ( 0.000000000000000000, -0.000000000000000000, -1.000000000000000000 ) ) ;
#12911 = DIRECTION ( 'NONE',  ( -1.000000000000000000, -0.000000000000000000, 0.000000000000000000 ) ) ;
#12912 = APPLICATION_PROTOCOL_DEFINITION ( 'draft international standard', 'automotive_design', 1998, #8064 ) ;
#12913 = CARTESIAN_POINT ( 'NONE',  ( -15.25966316918061949, 10.19618095414378800, -18.22035624981969093 ) ) ;
#12914 = ORIENTED_EDGE ( 'NONE', *, *, #6737, .F. ) ;
#12915 = DIRECTION ( 'NONE',  ( 1.000000000000000000, -0.000000000000000000, 0.000000000000000000 ) ) ;
#12916 = VECTOR ( 'NONE', #9772, 1000.000000000000000 ) ;
#12917 = CARTESIAN_POINT ( 'NONE',  ( 19.99999999999999645, 58.44960523466241398, -28.06621538408611016 ) ) ;
#12918 = CARTESIAN_POINT ( 'NONE',  ( -14.79893867793683349, -2.943691925285398359, -13.73482316848092744 ) ) ;
#12919 = FACE_OUTER_BOUND ( 'NONE', #3086, .T. ) ;
#12920 = APPLICATION_CONTEXT ( 'automotive_design' ) ;
#12921 = EDGE_CURVE ( 'NONE', #12993, #19867, #6329, .T. ) ;
#12922 = ORIENTED_EDGE ( 'NONE', *, *, #8684, .T. ) ;
#12923 = ADVANCED_FACE ( 'NONE', ( #5059 ), #12926, .F. ) ;
#12924 = DIRECTION ( 'NONE',  ( 1.000000000000000000, -0.000000000000000000, -0.000000000000000000 ) ) ;
#12925 = CARTESIAN_POINT ( 'NONE',  ( -7.500000000000007994, 1.491842755816071842, 21.07073125008779613 ) ) ;
#12926 = CYLINDRICAL_SURFACE ( 'NONE', #12438, 4.000000000000000000 ) ;
#12927 = ORIENTED_EDGE ( 'NONE', *, *, #18851, .F. ) ;
#12928 = VECTOR ( 'NONE', #17508, 999.9999999999998863 ) ;
#12929 = DIRECTION ( 'NONE',  ( -1.000000000000000000, 0.000000000000000000, -0.000000000000000000 ) ) ;
#12930 = AXIS2_PLACEMENT_3D ( 'NONE', #2253, #14975, #18155 ) ;
#12931 = ORIENTED_EDGE ( 'NONE', *, *, #18932, .F. ) ;
#12932 = LINE ( 'NONE', #9748, #4462 ) ;
#12933 = CARTESIAN_POINT ( 'NONE',  ( -6.888301780572500199, 16.62983158603121936, 18.45863750018030913 ) ) ;
#12934 = ORIENTED_EDGE ( 'NONE', *, *, #19695, .T. ) ;
#12935 = VECTOR ( 'NONE', #15870, 1000.000000000000000 ) ;
#12936 = EDGE_LOOP ( 'NONE', ( #3909, #18905, #13418, #12909 ) ) ;
#12937 = DIRECTION ( 'NONE',  ( 0.000000000000000000, -1.224646799147354686E-16, 1.000000000000000000 ) ) ;
#12938 =( NAMED_UNIT ( * ) SI_UNIT ( $, .STERADIAN. ) SOLID_ANGLE_UNIT ( ) );
#12939 = STYLED_ITEM ( 'NONE', ( #1957 ), #17573 ) ;
#12940 = LINE ( 'NONE', #19496, #2511 ) ;
#12941 = DIRECTION ( 'NONE',  ( -1.000000000000000000, -0.000000000000000000, -0.000000000000000000 ) ) ;
#12942 = CARTESIAN_POINT ( 'NONE',  ( 6.358192988180019434, 4.248408729364581582, 24.60510625018031661 ) ) ;
#12943 = AXIS2_PLACEMENT_3D ( 'NONE', #17614, #6371, #14338 ) ;
#12944 = CARTESIAN_POINT ( 'NONE',  ( 9.474249098604504482, 6.330490856366291830, -0.9387035002868041600 ) ) ;
#12945 = DIRECTION ( 'NONE',  ( -1.000000000000000000, 0.000000000000000000, 0.000000000000000000 ) ) ;
#12946 = AXIS2_PLACEMENT_3D ( 'NONE', #15162, #16638, #14954 ) ;
#12947 = DIRECTION ( 'NONE',  ( 0.000000000000000000, 0.000000000000000000, -1.000000000000000000 ) ) ;
#12948 = DIRECTION ( 'NONE',  ( 1.000000000000000000, 0.000000000000000000, 0.000000000000000000 ) ) ;
#12949 = VERTEX_POINT ( 'NONE', #4863 ) ;
#12950 = FACE_OUTER_BOUND ( 'NONE', #9141, .T. ) ;
#12951 = ORIENTED_EDGE ( 'NONE', *, *, #7519, .F. ) ;
#12952 = CARTESIAN_POINT ( 'NONE',  ( 12.72792205982779734, -12.72792206288791128, 15.06167500018031369 ) ) ;
#12953 = DIRECTION ( 'NONE',  ( 0.000000000000000000, 0.000000000000000000, -1.000000000000000000 ) ) ;
#12954 = ORIENTED_EDGE ( 'NONE', *, *, #9430, .T. ) ;
#12955 = CARTESIAN_POINT ( 'NONE',  ( -2.000000000000009770, 3.464101615137749057, 0.000000000000000000 ) ) ;
#12956 = EDGE_LOOP ( 'NONE', ( #2674, #16714, #10796, #6096 ) ) ;
#12957 = DIRECTION ( 'NONE',  ( 1.000000000000000000, 0.000000000000000000, 0.000000000000000000 ) ) ;
#12958 = LINE ( 'NONE', #329, #17845 ) ;
#12959 = ORIENTED_EDGE ( 'NONE', *, *, #7903, .F. ) ;
#12960 = ORIENTED_EDGE ( 'NONE', *, *, #18054, .F. ) ;
#12961 = LINE ( 'NONE', #3502, #13071 ) ;
#12962 = CIRCLE ( 'NONE', #3791, 65.24900000006525147 ) ;
#12963 = EDGE_CURVE ( 'NONE', #18514, #9743, #13029, .T. ) ;
#12964 = CIRCLE ( 'NONE', #19053, 27.60000000002759535 ) ;
#12965 = AXIS2_PLACEMENT_3D ( 'NONE', #16584, #5450, #1871 ) ;
#12966 = DIRECTION ( 'NONE',  ( 0.000000000000000000, 0.000000000000000000, 1.000000000000000000 ) ) ;
#12967 = LINE ( 'NONE', #6694, #20767 ) ;
#12968 = EDGE_CURVE ( 'NONE', #11336, #12652, #14615, .T. ) ;
#12969 = EDGE_LOOP ( 'NONE', ( #3782, #13078, #8390, #3091 ) ) ;
#12970 = CARTESIAN_POINT ( 'NONE',  ( -6.929096493489625530, 2.870125743571138255, 5.675362500180312075 ) ) ;
#12971 = CARTESIAN_POINT ( 'NONE',  ( 19.99999999999999645, 14.55863677812122425, 63.60407295269110506 ) ) ;
#12972 = AXIS2_PLACEMENT_3D ( 'NONE', #19777, #5259, #18199 ) ;
#12973 = CARTESIAN_POINT ( 'NONE',  ( 85.00002539999999840, 5.400000000000000355, 0.000000000000000000 ) ) ;
#12974 = PLANE ( 'NONE',  #5881 ) ;
#12975 = AXIS2_PLACEMENT_3D ( 'NONE', #13084, #16057, #11387 ) ;
#12976 = EDGE_LOOP ( 'NONE', ( #2915, #13517, #7277, #1846, #18564 ) ) ;
#12977 = DIRECTION ( 'NONE',  ( 1.000000000000000000, 0.000000000000000000, 0.000000000000000000 ) ) ;
#12978 = CARTESIAN_POINT ( 'NONE',  ( -17.99999999956958519, 3.580422614997674113, 16.98598125018031268 ) ) ;
#12979 = DIRECTION ( 'NONE',  ( -1.000000000000000000, 0.000000000000000000, 0.000000000000000000 ) ) ;
#12980 = ORIENTED_EDGE ( 'NONE', *, *, #7907, .T. ) ;
#12981 = FACE_OUTER_BOUND ( 'NONE', #17365, .T. ) ;
#12982 = VERTEX_POINT ( 'NONE', #6242 ) ;
#12983 = DIRECTION ( 'NONE',  ( -1.000000000000000000, -0.000000000000000000, 0.000000000000000000 ) ) ;
#12984 = CIRCLE ( 'NONE', #16689, 7.500000000000000000 ) ;
#12985 = EDGE_LOOP ( 'NONE', ( #18903, #15612, #2357, #11690, #15108, #17950, #20122, #11841, #16639, #10281, #12466, #11725, #18232, #15497 ) ) ;
#12986 = ADVANCED_FACE ( 'NONE', ( #6655 ), #9525, .T. ) ;
#12987 = ADVANCED_FACE ( 'NONE', ( #17806 ), #6546, .T. ) ;
#12988 = DIRECTION ( 'NONE',  ( -1.000000000000000000, -0.000000000000000000, -0.000000000000000000 ) ) ;
#12989 = AXIS2_PLACEMENT_3D ( 'NONE', #12568, #19034, #4509 ) ;
#12990 = EDGE_CURVE ( 'NONE', #7867, #13475, #3275, .T. ) ;
#12991 = CARTESIAN_POINT ( 'NONE',  ( 19.99999999999999645, 48.70996102988680576, 42.79495875147792106 ) ) ;
#12992 = CARTESIAN_POINT ( 'NONE',  ( -11.17563879758428769, -2.222972768810840272, 20.91057850064743207 ) ) ;
#12993 = VERTEX_POINT ( 'NONE', #16404 ) ;
#12994 = CARTESIAN_POINT ( 'NONE',  ( 19.99999999999999645, 0.000000000000000000, 0.000000000000000000 ) ) ;
#12995 = DIRECTION ( 'NONE',  ( -1.000000000000000000, -0.000000000000000000, 0.000000000000000000 ) ) ;
#12996 = VERTEX_POINT ( 'NONE', #14419 ) ;
#12997 = CYLINDRICAL_SURFACE ( 'NONE', #10829, 72.00000000007199219 ) ;
#12998 = CIRCLE ( 'NONE', #5185, 2.649999999999999467 ) ;
#12999 = AXIS2_PLACEMENT_3D ( 'NONE', #10854, #15731, #3621 ) ;
#13000 = CARTESIAN_POINT ( 'NONE',  ( -6.888301784570738384, -16.62983158437509346, 16.82886250018031404 ) ) ;
#13001 = CARTESIAN_POINT ( 'NONE',  ( 6.249999999999902300, -10.82531754730554496, 166.0000000000000000 ) ) ;
#13002 = DIRECTION ( 'NONE',  ( -1.000000000000000000, -0.000000000000000000, -0.000000000000000000 ) ) ;
#13003 = EDGE_CURVE ( 'NONE', #9313, #8953, #11416, .T. ) ;
#13004 = AXIS2_PLACEMENT_3D ( 'NONE', #1729, #10090, #3408 ) ;
#13005 = AXIS2_PLACEMENT_3D ( 'NONE', #4585, #19112, #10941 ) ;
#13006 = ADVANCED_FACE ( 'NONE', ( #3172 ), #16205, .F. ) ;
#13007 = ORIENTED_EDGE ( 'NONE', *, *, #2852, .T. ) ;
#13008 = VECTOR ( 'NONE', #16458, 1000.000000000000000 ) ;
#13009 = CARTESIAN_POINT ( 'NONE',  ( 2.500000000000000000, 0.000000000000000000, 0.000000000000000000 ) ) ;
#13010 = ORIENTED_EDGE ( 'NONE', *, *, #10958, .T. ) ;
#13011 = CARTESIAN_POINT ( 'NONE',  ( 0.000000000000000000, 1.178949249685217415, 2.041999999999998483 ) ) ;
#13012 = CARTESIAN_POINT ( 'NONE',  ( -9.850000000000012079, 3.245314017740478073E-16, 166.0000000000000000 ) ) ;
#13013 = CARTESIAN_POINT ( 'NONE',  ( 10.19618095047497697, -15.25966317163202923, -24.24839374981969087 ) ) ;
#13014 = ADVANCED_FACE ( 'NONE', ( #1597 ), #8051, .T. ) ;
#13015 = VERTEX_POINT ( 'NONE', #2405 ) ;
#13016 = CARTESIAN_POINT ( 'NONE',  ( 19.99999999999999645, -27.80658314415271093, 66.41380830714113870 ) ) ;
#13017 = DIRECTION ( 'NONE',  ( 0.000000000000000000, 0.000000000000000000, -1.000000000000000000 ) ) ;
#13018 = VECTOR ( 'NONE', #341, 1000.000000000000000 ) ;
#13019 = CARTESIAN_POINT ( 'NONE',  ( -3.580422610670018990, 18.00000000043041481, -7.617231249819690575 ) ) ;
#13020 = ORIENTED_EDGE ( 'NONE', *, *, #14772, .T. ) ;
#13021 = VECTOR ( 'NONE', #11661, 1000.000000000000000 ) ;
#13022 = CARTESIAN_POINT ( 'NONE',  ( 0.000000000000000000, 0.000000000000000000, 0.000000000000000000 ) ) ;
#13023 = CARTESIAN_POINT ( 'NONE',  ( 0.000000000000000000, 0.000000000000000000, 0.000000000000000000 ) ) ;
#13024 = CARTESIAN_POINT ( 'NONE',  ( 10.46442989454075168, 10.46442989202483886, -9.905916918480928146 ) ) ;
#13025 = ORIENTED_EDGE ( 'NONE', *, *, #1359, .T. ) ;
#13026 = VERTEX_POINT ( 'NONE', #3772 ) ;
#13027 = CARTESIAN_POINT ( 'NONE',  ( 19.99999999999999645, 35.35772184876879720, 54.34979580218204376 ) ) ;
#13028 = CARTESIAN_POINT ( 'NONE',  ( 7.500000000179346316, 1.491842754445843244, 25.19416875018031732 ) ) ;
#13029 = LINE ( 'NONE', #17699, #3295 ) ;
#13030 = EDGE_LOOP ( 'NONE', ( #1392, #18742, #7946, #9354, #1413, #11766 ) ) ;
#13031 = DIRECTION ( 'NONE',  ( 0.000000000000000000, -0.1361666490962538945, 0.9906859460363297565 ) ) ;
#13032 = ORIENTED_EDGE ( 'NONE', *, *, #17967, .T. ) ;
#13033 = PRESENTATION_LAYER_ASSIGNMENT (  '', '', ( #8628 ) ) ;
#13034 = CYLINDRICAL_SURFACE ( 'NONE', #6481, 80.00000000000000000 ) ;
#13035 = CARTESIAN_POINT ( 'NONE',  ( 6.888301784570727726, 16.62983158437509701, 19.63676250018031411 ) ) ;
#13036 = ORIENTED_EDGE ( 'NONE', *, *, #7007, .T. ) ;
#13037 = EDGE_LOOP ( 'NONE', ( #3751, #435, #5654, #9993 ) ) ;
#13038 = DIRECTION ( 'NONE',  ( 0.000000000000000000, 0.000000000000000000, 1.000000000000000000 ) ) ;
#13039 = DIRECTION ( 'NONE',  ( 0.000000000000000000, 0.000000000000000000, 1.000000000000000000 ) ) ;
#13040 = FILL_AREA_STYLE ('',( #11647 ) ) ;
#13041 =( GEOMETRIC_REPRESENTATION_CONTEXT ( 3 ) GLOBAL_UNCERTAINTY_ASSIGNED_CONTEXT ( ( #4105 ) ) GLOBAL_UNIT_ASSIGNED_CONTEXT ( ( #6532, #11422, #1682 ) ) REPRESENTATION_CONTEXT ( 'NONE', 'WORKASPACE' ) );
#13042 = CARTESIAN_POINT ( 'NONE',  ( -24.99999999999999289, 31.35083268962915426, 84.99999999999998579 ) ) ;
#13043 = ADVANCED_FACE ( 'NONE', ( #5575 ), #5161, .F. ) ;
#13044 = DIRECTION ( 'NONE',  ( 1.000000000000000000, 0.000000000000000000, 0.000000000000000000 ) ) ;
#13045 = CARTESIAN_POINT ( 'NONE',  ( 6.330490856366294494, -9.474249098604513364, -19.73473399935257788 ) ) ;
#13046 = CIRCLE ( 'NONE', #3884, 27.60000000002759535 ) ;
#13047 = CARTESIAN_POINT ( 'NONE',  ( -9.474249097082497073, 6.330490858644137298, -3.884016000286802495 ) ) ;
#13048 = CARTESIAN_POINT ( 'NONE',  ( 50.00000000000000000, -105.0000000000000284, -77.45966692414833688 ) ) ;
#13049 = DIRECTION ( 'NONE',  ( -1.000000000000000000, 0.000000000000000000, 0.000000000000000000 ) ) ;
#13050 = EDGE_LOOP ( 'NONE', ( #9534, #7976, #18974, #16606 ) ) ;
#13051 = DIRECTION ( 'NONE',  ( -1.000000000000000000, -0.000000000000000000, 0.000000000000000000 ) ) ;
#13052 = CARTESIAN_POINT ( 'NONE',  ( -15.25966316918061771, 10.19618095414378622, 19.47964375018031546 ) ) ;
#13053 = CARTESIAN_POINT ( 'NONE',  ( 2.500000000000000000, 2.357898499370433054, -1.951563910473907981E-15 ) ) ;
#13054 = ORIENTED_EDGE ( 'NONE', *, *, #18542, .F. ) ;
#13055 = DIRECTION ( 'NONE',  ( 1.000000000000000000, 0.000000000000000000, 0.000000000000000000 ) ) ;
#13056 = EDGE_LOOP ( 'NONE', ( #133, #4047, #16765, #18617 ) ) ;
#13057 = DIRECTION ( 'NONE',  ( 0.000000000000000000, 0.000000000000000000, -1.000000000000000000 ) ) ;
#13058 = DIRECTION ( 'NONE',  ( 0.000000000000000000, 0.000000000000000000, -1.000000000000000000 ) ) ;
#13059 = AXIS2_PLACEMENT_3D ( 'NONE', #6732, #14596, #13114 ) ;
#13060 = ORIENTED_EDGE ( 'NONE', *, *, #9782, .F. ) ;
#13061 = ORIENTED_EDGE ( 'NONE', *, *, #20901, .T. ) ;
#13062 = CARTESIAN_POINT ( 'NONE',  ( -10.00000000000000000, 0.000000000000000000, 0.000000000000000000 ) ) ;
#13063 = VECTOR ( 'NONE', #20469, 1000.000000000000000 ) ;
#13064 = SHAPE_REPRESENTATION ( 'spur gear_iso_ISO - Spur gear 3M 46T 20PA 20FW ---S46C15H150L8.0S1', ( #12461 ), #5631 ) ;
#13065 = SURFACE_STYLE_FILL_AREA ( #9974 ) ;
#13066 = CARTESIAN_POINT ( 'NONE',  ( 19.99999999999999645, 63.05226888949912478, -15.11556105343395906 ) ) ;
#13067 = EDGE_CURVE ( 'NONE', #8003, #520, #8890, .T. ) ;
#13068 = DIRECTION ( 'NONE',  ( 0.000000000000000000, 0.000000000000000000, 1.000000000000000000 ) ) ;
#13069 = ORIENTED_EDGE ( 'NONE', *, *, #15009, .F. ) ;
#13070 = CARTESIAN_POINT ( 'NONE',  ( -4.248408730893245000, -6.358192987158590270, 13.03864375018031296 ) ) ;
#13071 = VECTOR ( 'NONE', #1827, 1000.000000000000000 ) ;
#13072 = FACE_OUTER_BOUND ( 'NONE', #13964, .T. ) ;
#13073 = DIRECTION ( 'NONE',  ( -1.000000000000000000, 0.000000000000000000, 0.000000000000000000 ) ) ;
#13074 = CYLINDRICAL_SURFACE ( 'NONE', #8573, 2.099999999999997868 ) ;
#13075 = ADVANCED_FACE ( 'NONE', ( #8864, #11840 ), #3880, .T. ) ;
#13076 = AXIS2_PLACEMENT_3D ( 'NONE', #15520, #906, #13837 ) ;
#13077 = AXIS2_PLACEMENT_3D ( 'NONE', #9406, #1357, #1671 ) ;
#13078 = ORIENTED_EDGE ( 'NONE', *, *, #16005, .T. ) ;
#13079 = DIRECTION ( 'NONE',  ( 0.000000000000000000, 0.000000000000000000, -1.000000000000000000 ) ) ;
#13080 = VERTEX_POINT ( 'NONE', #16716 ) ;
#13081 = CARTESIAN_POINT ( 'NONE',  ( -12.72792206288791128, -12.72792205982779912, 15.51332500018031624 ) ) ;
#13082 = DIRECTION ( 'NONE',  ( -0.000000000000000000, -1.000000000000000000, -0.000000000000000000 ) ) ;
#13083 = ORIENTED_EDGE ( 'NONE', *, *, #2989, .F. ) ;
#13084 = CARTESIAN_POINT ( 'NONE',  ( 19.99999999999999645, 64.79224928664386596, 2.456263514198732345 ) ) ;
#13085 = ORIENTED_EDGE ( 'NONE', *, *, #18940, .F. ) ;
#13086 = CARTESIAN_POINT ( 'NONE',  ( 6.232799999999996565, 0.000000000000000000, 10.79377999999999993 ) ) ;
#13087 = CIRCLE ( 'NONE', #3922, 2.649999999999992806 ) ;
#13088 = VERTEX_POINT ( 'NONE', #396 ) ;
#13089 = CIRCLE ( 'NONE', #4297, 65.24900000006525147 ) ;
#13090 = CARTESIAN_POINT ( 'NONE',  ( -15.15000000000000036, 0.000000000000000000, 126.0000000000000000 ) ) ;
#13091 = AXIS2_PLACEMENT_3D ( 'NONE', #1125, #2913, #17644 ) ;
#13092 = PRESENTATION_LAYER_ASSIGNMENT (  '', '', ( #10737 ) ) ;
#13093 = DIRECTION ( 'NONE',  ( -1.000000000000000000, 0.000000000000000000, 0.000000000000000000 ) ) ;
#13094 = CARTESIAN_POINT ( 'NONE',  ( -7.902369978624331104, -7.902369976724401113, 20.02698475064743278 ) ) ;
#13095 = ORIENTED_EDGE ( 'NONE', *, *, #12344, .T. ) ;
#13096 = CARTESIAN_POINT ( 'NONE',  ( 24.99999999999999645, -122.0000000000000000, -6.368163355566234804E-15 ) ) ;
#13097 = EDGE_CURVE ( 'NONE', #11, #14849, #6850, .T. ) ;
#13098 = CARTESIAN_POINT ( 'NONE',  ( 0.000000000000000000, 0.000000000000000000, 166.0000000000000000 ) ) ;
#13099 = ORIENTED_EDGE ( 'NONE', *, *, #5729, .T. ) ;
#13100 = FACE_OUTER_BOUND ( 'NONE', #2590, .T. ) ;
#13101 = EDGE_CURVE ( 'NONE', #20455, #7012, #16957, .T. ) ;
#13102 = AXIS2_PLACEMENT_3D ( 'NONE', #10033, #4950, #4847 ) ;
#13103 = EDGE_CURVE ( 'NONE', #2180, #16859, #14924, .T. ) ;
#13104 = CARTESIAN_POINT ( 'NONE',  ( 19.99999999999999645, 61.72688495901613948, -19.84591825364033468 ) ) ;
#13105 = DIRECTION ( 'NONE',  ( 0.000000000000000000, -0.5000000000000009992, -0.8660254037844380415 ) ) ;
#13106 = AXIS2_PLACEMENT_3D ( 'NONE', #709, #6849, #13339 ) ;
#13107 = VERTEX_POINT ( 'NONE', #19788 ) ;
#13108 = VECTOR ( 'NONE', #12399, 1000.000000000000000 ) ;
#13109 = CARTESIAN_POINT ( 'NONE',  ( 2.500000000000002220, 0.000000000000000000, -5.600000000000000533 ) ) ;
#13110 = EDGE_CURVE ( 'NONE', #3529, #13866, #19666, .T. ) ;
#13111 = ORIENTED_EDGE ( 'NONE', *, *, #7903, .T. ) ;
#13112 = PRODUCT_RELATED_PRODUCT_CATEGORY ( 'part', '', ( #10346 ) ) ;
#13113 = CYLINDRICAL_SURFACE ( 'NONE', #12965, 2.650000000000000355 ) ;
#13114 = DIRECTION ( 'NONE',  ( 0.000000000000000000, 0.000000000000000000, -1.000000000000000000 ) ) ;
#13115 = CARTESIAN_POINT ( 'NONE',  ( -6.888301784570736608, -16.62983158437509346, -22.77573749981969087 ) ) ;
#13116 = CIRCLE ( 'NONE', #16498, 50.00000000000001421 ) ;
#13117 = ORIENTED_EDGE ( 'NONE', *, *, #17932, .F. ) ;
#13118 = DIRECTION ( 'NONE',  ( 0.000000000000000000, 0.000000000000000000, 1.000000000000000000 ) ) ;
#13119 = AXIS2_PLACEMENT_3D ( 'NONE', #20926, #4819, #3027 ) ;
#13120 = DIRECTION ( 'NONE',  ( -0.000000000000000000, -0.000000000000000000, 1.000000000000000000 ) ) ;
#13121 = SHAPE_DEFINITION_REPRESENTATION ( #531, #13739 ) ;
#13122 = CARTESIAN_POINT ( 'NONE',  ( 16.62983158437509701, -6.888301784570740161, -4.377387499819692884 ) ) ;
#13123 = EDGE_CURVE ( 'NONE', #1189, #10440, #3676, .T. ) ;
#13125 = ORIENTED_EDGE ( 'NONE', *, *, #11555, .F. ) ;
#13124 = AXIS2_PLACEMENT_3D ( 'NONE', #2999, #9458, #15919 ) ;
#13126 = AXIS2_PLACEMENT_3D ( 'NONE', #795, #2380, #7357 ) ;
#13127 = CARTESIAN_POINT ( 'NONE',  ( 20.00000000000000000, 0.000000000000000000, 0.000000000000000000 ) ) ;
#13128 = CARTESIAN_POINT ( 'NONE',  ( 19.99999999999999645, 0.000000000000000000, 0.000000000000000000 ) ) ;
#13129 = EDGE_CURVE ( 'NONE', #510, #11587, #6959, .T. ) ;
#13130 = CARTESIAN_POINT ( 'NONE',  ( 5.663308646854338768, -13.67243654778934747, 2.464395581519073897 ) ) ;
#13131 = EDGE_CURVE ( 'NONE', #16859, #9681, #12099, .T. ) ;
#13132 = LINE ( 'NONE', #3269, #12270 ) ;
#13133 = CIRCLE ( 'NONE', #15838, 72.00000000007199219 ) ;
#13134 = EDGE_CURVE ( 'NONE', #4444, #12032, #1150, .T. ) ;
#13135 = ORIENTED_EDGE ( 'NONE', *, *, #2892, .F. ) ;
#13136 = FACE_OUTER_BOUND ( 'NONE', #13563, .T. ) ;
#13137 = CIRCLE ( 'NONE', #4674, 2.099999999999997868 ) ;
#13138 = CARTESIAN_POINT ( 'NONE',  ( 30.00000000000000000, -85.00000000000000000, -1.040949779275250179E-14 ) ) ;
#13139 = CARTESIAN_POINT ( 'NONE',  ( 34.94904587705838850, -25.30803235969634457, 69.13077653488730334 ) ) ;
#13140 = VERTEX_POINT ( 'NONE', #2523 ) ;
#13141 = CARTESIAN_POINT ( 'NONE',  ( 19.99999999999999645, 65.23577793412344761, 1.313498510941937036 ) ) ;
#13142 = ORIENTED_EDGE ( 'NONE', *, *, #11594, .T. ) ;
#13143 = FACE_BOUND ( 'NONE', #1719, .T. ) ;
#13144 = DIRECTION ( 'NONE',  ( 1.000000000000000000, 0.000000000000000000, 0.000000000000000000 ) ) ;
#13145 = ORIENTED_EDGE ( 'NONE', *, *, #8321, .F. ) ;
#13146 = ORIENTED_EDGE ( 'NONE', *, *, #9613, .F. ) ;
#13147 = FACE_OUTER_BOUND ( 'NONE', #17744, .T. ) ;
#13148 = DIRECTION ( 'NONE',  ( 0.000000000000000000, 0.8878852184023731109, 0.4600650377311562012 ) ) ;
#13149 = DIRECTION ( 'NONE',  ( 1.000000000000000000, 0.000000000000000000, 0.000000000000000000 ) ) ;
#13150 = EDGE_CURVE ( 'NONE', #13592, #6079, #9737, .T. ) ;
#13151 = CARTESIAN_POINT ( 'NONE',  ( -17.50000000000000355, 2.143131898507868643E-15, 166.0000000000000000 ) ) ;
#13152 = CARTESIAN_POINT ( 'NONE',  ( -5.303300858261589035, 5.303300859536635770, 12.52932500018031448 ) ) ;
#13153 = CARTESIAN_POINT ( 'NONE',  ( 11.17563879731704723, -1.343450868547281106E-09, -0.05510975028680254600 ) ) ;
#13154 = LINE ( 'NONE', #14439, #15397 ) ;
#13155 = CYLINDRICAL_SURFACE ( 'NONE', #14433, 2.099999999999997868 ) ;
#13156 = EDGE_LOOP ( 'NONE', ( #94, #8977, #1674, #20043 ) ) ;
#13157 = DIRECTION ( 'NONE',  ( -0.000000000000000000, -0.000000000000000000, -1.000000000000000000 ) ) ;
#13158 = CARTESIAN_POINT ( 'NONE',  ( 18.00000000000000000, -2.163824016901520184E-09, -25.72104999981969087 ) ) ;
#13159 = DIRECTION ( 'NONE',  ( -1.000000000000000000, 0.000000000000000000, 0.000000000000000000 ) ) ;
#13160 = VERTEX_POINT ( 'NONE', #7381 ) ;
#13161 = DIRECTION ( 'NONE',  ( 1.000000000000000000, 0.000000000000000000, 0.000000000000000000 ) ) ;
#13162 = VERTEX_POINT ( 'NONE', #12261 ) ;
#13163 = DIRECTION ( 'NONE',  ( 1.000000000000000000, 0.000000000000000000, 0.000000000000000000 ) ) ;
#13164 = DIRECTION ( 'NONE',  ( 0.000000000000000000, -0.4999999999999989453, 0.8660254037844391517 ) ) ;
#13165 = B_SPLINE_CURVE_WITH_KNOTS ( 'NONE', 3,
 ( #18439, #13360, #8574, #18126 ),
 .UNSPECIFIED., .F., .F.,
 ( 4, 4 ),
 ( 2.380737581782212780E-07, 0.002336974151641539946 ),
 .UNSPECIFIED. ) ;
#13166 = EDGE_CURVE ( 'NONE', #10361, #7721, #9092, .T. ) ;
#13167 = EDGE_LOOP ( 'NONE', ( #18253, #19075, #13327, #6996 ) ) ;
#13168 = ORIENTED_EDGE ( 'NONE', *, *, #355, .F. ) ;
#13169 = CARTESIAN_POINT ( 'NONE',  ( 30.00000000000000000, -99.99999999999998579, 52.00000000000000000 ) ) ;
#13170 = SURFACE_STYLE_FILL_AREA ( #14859 ) ;
#13171 = CARTESIAN_POINT ( 'NONE',  ( 0.000000000000000000, 0.000000000000000000, 0.000000000000000000 ) ) ;
#13172 = FACE_OUTER_BOUND ( 'NONE', #11838, .T. ) ;
#13173 = ORIENTED_EDGE ( 'NONE', *, *, #16847, .T. ) ;
#13174 = CARTESIAN_POINT ( 'NONE',  ( -7.500000000000000888, 9.015942588607330751E-10, 14.51130000018031119 ) ) ;
#13175 = CARTESIAN_POINT ( 'NONE',  ( 30.00000000000000000, -105.0000000000000000, -77.45966692414833688 ) ) ;
#13176 = SURFACE_STYLE_USAGE ( .BOTH. , #13583 ) ;
#13177 = CARTESIAN_POINT ( 'NONE',  ( -44.00000000000000000, -85.00000000000000000, 14.49999999999998579 ) ) ;
#13178 = CARTESIAN_POINT ( 'NONE',  ( 17.00000000000000000, 2.055000000000000160, 0.000000000000000000 ) ) ;
#13179 = VECTOR ( 'NONE', #1619, 1000.000000000000000 ) ;
#13180 = ORIENTED_EDGE ( 'NONE', *, *, #5970, .F. ) ;
#13181 = CARTESIAN_POINT ( 'NONE',  ( -24.99999999999999289, -85.00000000000000000, -1.040949779275250179E-14 ) ) ;
#13182 = VERTEX_POINT ( 'NONE', #7714 ) ;
#13183 = CARTESIAN_POINT ( 'NONE',  ( -6.888301780572501976, 16.62983158603122291, 18.45863750018031268 ) ) ;
#13184 = CARTESIAN_POINT ( 'NONE',  ( -44.00000000000000000, -85.00000000000000000, -1.040949779275250179E-14 ) ) ;
#13185 = ORIENTED_EDGE ( 'NONE', *, *, #19984, .F. ) ;
#13186 = FACE_OUTER_BOUND ( 'NONE', #20257, .T. ) ;
#13187 = VERTEX_POINT ( 'NONE', #20206 ) ;
#13188 = CYLINDRICAL_SURFACE ( 'NONE', #5754, 27.60000000002759535 ) ;
#13189 = FACE_BOUND ( 'NONE', #1767, .T. ) ;
#13190 = ADVANCED_FACE ( 'NONE', ( #8980 ), #4417, .F. ) ;
#13191 =( BOUNDED_CURVE ( )  B_SPLINE_CURVE ( 2, ( #3894, #16937, #8772, #3999, #6866, #7074, #13554, #20000, #12169, #16733, #5484, #13461, #5283, #19907, #18544, #2212, #18320 ),
 .UNSPECIFIED., .F., .F. ) 
 B_SPLINE_CURVE_WITH_KNOTS ( ( 3, 2, 2, 2, 2, 2, 2, 2, 3 ),
 ( 0.8000000000038511860, 0.8125000000038511416, 0.8250000000038510972, 0.8375000000038511638, 0.8500000000038511194, 0.8625000000038511860, 0.8750000000038511416, 0.8875000000038510972, 0.9000000000038511638 ),
 .UNSPECIFIED. ) 
 CURVE ( )  GEOMETRIC_REPRESENTATION_ITEM ( )  RATIONAL_B_SPLINE_CURVE ( ( 0.9999999999940800688, 0.9807852804091503618, 1.000000000000000000, 0.9807852804032304306, 1.000000000000000000, 0.9807852804032304306, 1.000000000000000000, 0.9807852804032304306, 1.000000000000000000, 0.9807852804032304306, 1.000000000000000000, 0.9807852804032304306, 1.000000000000000000, 0.9807852804032304306, 1.000000000000000000, 0.9807852803973104994, 1.000000000005919931 ) ) 
 REPRESENTATION_ITEM ( '' )  );
#13192 = ORIENTED_EDGE ( 'NONE', *, *, #5389, .F. ) ;
#13193 = CARTESIAN_POINT ( 'NONE',  ( -24.99999999999999289, -85.00000000000000000, -1.040949779275250179E-14 ) ) ;
#13194 = VECTOR ( 'NONE', #7265, 1000.000000000000000 ) ;
#13195 = DIRECTION ( 'NONE',  ( 0.000000000000000000, 0.000000000000000000, -1.000000000000000000 ) ) ;
#13196 = CARTESIAN_POINT ( 'NONE',  ( -9.474249097082500626, 6.330490858644140850, 3.238703500647428957 ) ) ;
#13197 = EDGE_LOOP ( 'NONE', ( #9774, #1743, #13293, #9279 ) ) ;
#13198 = CARTESIAN_POINT ( 'NONE',  ( -2.000000000000022649, -3.464101615137742396, -5.600000000000000533 ) ) ;
#13199 = CARTESIAN_POINT ( 'NONE',  ( 0.000000000000000000, 0.000000000000000000, -90.00000000000000000 ) ) ;
#13200 = ORIENTED_EDGE ( 'NONE', *, *, #16316, .F. ) ;
#13201 = DIRECTION ( 'NONE',  ( -1.000000000000000000, -0.000000000000000000, -0.000000000000000000 ) ) ;
#13202 = EDGE_LOOP ( 'NONE', ( #17987, #1104, #20817, #10835 ) ) ;
#13203 = CARTESIAN_POINT ( 'NONE',  ( 18.00000000043041126, 3.580422610670019434, 23.01401875018031262 ) ) ;
#13204 = DIRECTION ( 'NONE',  ( -1.000000000000000000, -0.000000000000000000, -0.000000000000000000 ) ) ;
#13205 = DIRECTION ( 'NONE',  ( 0.000000000000000000, 0.9790840876823234673, -0.2034560130526309185 ) ) ;
#13206 = EDGE_LOOP ( 'NONE', ( #17943, #3397, #7579, #7879 ) ) ;
#13207 = CARTESIAN_POINT ( 'NONE',  ( 19.99999999999999645, -64.52323195238624010, -6.389157729493822657 ) ) ;
#13208 = ORIENTED_EDGE ( 'NONE', *, *, #18651, .T. ) ;
#13209 = CARTESIAN_POINT ( 'NONE',  ( -15.15000000000000036, 3.245314017740478073E-16, 46.00000000000000711 ) ) ;
#13210 = CARTESIAN_POINT ( 'NONE',  ( -5.303300859536636658, -5.303300858261589035, -18.10192499981969050 ) ) ;
#13211 = VECTOR ( 'NONE', #6792, 1000.000000000000000 ) ;
#13212 = EDGE_LOOP ( 'NONE', ( #18705, #497, #19124, #12552 ) ) ;
#13213 = DIRECTION ( 'NONE',  ( 0.000000000000000000, 0.000000000000000000, -1.000000000000000000 ) ) ;
#13214 = ADVANCED_FACE ( 'NONE', ( #12377, #15447, #18738, #2831, #6013 ), #937, .T. ) ;
#13215 = PRODUCT ( 'output shaft', 'output shaft', '', ( #10036 ) ) ;
#13216 = EDGE_CURVE ( 'NONE', #10156, #10605, #10790, .T. ) ;
#13217 = DIRECTION ( 'NONE',  ( 1.000000000000000000, 1.836909530733573776E-16, 0.000000000000000000 ) ) ;
#13218 = APPLICATION_PROTOCOL_DEFINITION ( 'draft international standard', 'automotive_design', 1998, #18739 ) ;
#13219 = CARTESIAN_POINT ( 'NONE',  ( -12.72792205982780089, 12.72792206288791128, -17.92582499981969235 ) ) ;
#13220 = ORIENTED_EDGE ( 'NONE', *, *, #11106, .F. ) ;
#13221 = CARTESIAN_POINT ( 'NONE',  ( 7.500000000000000888, -2.290195989456150567E-15, 9.798800000002307442 ) ) ;
#13222 = EDGE_CURVE ( 'NONE', #13237, #1377, #13087, .T. ) ;
#13223 = CYLINDRICAL_SURFACE ( 'NONE', #9746, 65.24900000006525147 ) ;
#13224 = CARTESIAN_POINT ( 'NONE',  ( 12.54593441764186679, 8.382925368423272516, -0.1863856684809275799 ) ) ;
#13225 = EDGE_LOOP ( 'NONE', ( #8378, #8720 ) ) ;
#13226 = VECTOR ( 'NONE', #6163, 1000.000000000000000 ) ;
#13227 = DIRECTION ( 'NONE',  ( 0.000000000000000000, 0.000000000000000000, 1.000000000000000000 ) ) ;
#13228 = FACE_OUTER_BOUND ( 'NONE', #13156, .T. ) ;
#13229 = CARTESIAN_POINT ( 'NONE',  ( -6.929096493489627306, 2.870125743571138699, 15.10036250018031012 ) ) ;
#13230 = ORIENTED_EDGE ( 'NONE', *, *, #292, .F. ) ;
#13231 = ADVANCED_FACE ( 'NONE', ( #5907 ), #18886, .T. ) ;
#13232 = CARTESIAN_POINT ( 'NONE',  ( -5.303300859536636658, -5.303300858261589035, 10.17307500018031519 ) ) ;
#13233 = EDGE_LOOP ( 'NONE', ( #16554, #3797, #19407, #6592, #13823, #20019 ) ) ;
#13234 = DIRECTION ( 'NONE',  ( 0.000000000000000000, 0.000000000000000000, -1.000000000000000000 ) ) ;
#13235 = DIRECTION ( 'NONE',  ( 0.000000000000000000, 0.000000000000000000, -1.000000000000000000 ) ) ;
#13236 = ORIENTED_EDGE ( 'NONE', *, *, #4792, .T. ) ;
#13237 = VERTEX_POINT ( 'NONE', #18948 ) ;
#13238 = CARTESIAN_POINT ( 'NONE',  ( -24.99999999999999289, 31.35083268962915426, 50.63110039191614220 ) ) ;
#13239 = ADVANCED_FACE ( 'NONE', ( #20422 ), #12156, .T. ) ;
#13240 = EDGE_CURVE ( 'NONE', #11744, #11554, #6343, .T. ) ;
#13241 = CARTESIAN_POINT ( 'NONE',  ( 0.000000000000000000, 71.76067541710858677, -5.865617076723870227 ) ) ;
#13242 = CYLINDRICAL_SURFACE ( 'NONE', #15303, 2.649999999999999467 ) ;
#13243 = AXIS2_PLACEMENT_3D ( 'NONE', #14212, #2663, #7837 ) ;
#13244 = CARTESIAN_POINT ( 'NONE',  ( 0.000000000000000000, -46.01927912072495275, -45.67597560296436399 ) ) ;
#13245 = UNCERTAINTY_MEASURE_WITH_UNIT (LENGTH_MEASURE( 1.000000000000000082E-05 ), #16006, 'distance_accuracy_value', 'NONE');
#13247 = EDGE_CURVE ( 'NONE', #18653, #19379, #2942, .T. ) ;
#13246 = CARTESIAN_POINT ( 'NONE',  ( 19.99999999999999645, 0.000000000000000000, 0.000000000000000000 ) ) ;
#13248 = CARTESIAN_POINT ( 'NONE',  ( -9.015947181032835626E-10, -7.500000000000007994, 8.994950000180315541 ) ) ;
#13249 = CARTESIAN_POINT ( 'NONE',  ( -1.343452921478823292E-09, -11.17563879731704723, 11.72614024971320212 ) ) ;
#13250 = DIRECTION ( 'NONE',  ( 0.000000000000000000, 0.000000000000000000, 1.000000000000000000 ) ) ;
#13251 = DIRECTION ( 'NONE',  ( -0.000000000000000000, 0.000000000000000000, 1.000000000000000000 ) ) ;
#13252 = CIRCLE ( 'NONE', #13955, 65.24900000006525147 ) ;
#13253 = EDGE_CURVE ( 'NONE', #20655, #10422, #8046, .T. ) ;
#13254 = EDGE_LOOP ( 'NONE', ( #17092, #13944, #7942, #7416 ) ) ;
#13255 = DIRECTION ( 'NONE',  ( -1.551631016079434906E-16, 1.000000000000000000, 0.000000000000000000 ) ) ;
#13256 = CARTESIAN_POINT ( 'NONE',  ( -18.00000000000000000, 2.163826221265758884E-09, 9.171050000180313688 ) ) ;
#13257 = CARTESIAN_POINT ( 'NONE',  ( 52.50000000000000000, -120.0000000000000142, 5.000000000000000000 ) ) ;
#13258 = AXIS2_PLACEMENT_3D ( 'NONE', #19900, #5376, #10259 ) ;
#13259 = ADVANCED_FACE ( 'NONE', ( #17355 ), #14188, .F. ) ;
#13260 = ORIENTED_EDGE ( 'NONE', *, *, #6737, .T. ) ;
#13261 = EDGE_CURVE ( 'NONE', #7112, #964, #13707, .T. ) ;
#13262 = DIRECTION ( 'NONE',  ( 1.000000000000000000, -0.000000000000000000, -0.000000000000000000 ) ) ;
#13263 = VERTEX_POINT ( 'NONE', #20630 ) ;
#13264 = DIRECTION ( 'NONE',  ( 0.000000000000000000, 0.4999999999999993339, -0.8660254037844390407 ) ) ;
#13265 = CARTESIAN_POINT ( 'NONE',  ( 2.500000000000000000, -2.357898499370432166, 3.035766082959412415E-15 ) ) ;
#13266 = ORIENTED_EDGE ( 'NONE', *, *, #3058, .F. ) ;
#13267 = EDGE_LOOP ( 'NONE', ( #17931, #4955, #5328, #4563 ) ) ;
#13268 = DIRECTION ( 'NONE',  ( -1.000000000000000000, -0.000000000000000000, -0.000000000000000000 ) ) ;
#13269 = EDGE_CURVE ( 'NONE', #2640, #3338, #4951, .T. ) ;
#13270 = CARTESIAN_POINT ( 'NONE',  ( 9.999999999999998224, 51.96384592647267908, -49.83732252579563493 ) ) ;
#13271 = VECTOR ( 'NONE', #11084, 1000.000000000000000 ) ;
#13272 = AXIS2_PLACEMENT_3D ( 'NONE', #17752, #3221, #9689 ) ;
#13273 = DIRECTION ( 'NONE',  ( -1.000000000000000000, 0.000000000000000000, -0.000000000000000000 ) ) ;
#13274 = AXIS2_PLACEMENT_3D ( 'NONE', #15682, #6136, #12184 ) ;
#13275 = CARTESIAN_POINT ( 'NONE',  ( 2.870125743571137811, 6.929096493489625530, 8.031612500180312253 ) ) ;
#13276 = FACE_OUTER_BOUND ( 'NONE', #16114, .T. ) ;
#13277 = CYLINDRICAL_SURFACE ( 'NONE', #7096, 72.00000000007199219 ) ;
#13278 = LINE ( 'NONE', #12973, #14040 ) ;
#13279 = DIRECTION ( 'NONE',  ( 0.000000000000000000, 0.000000000000000000, -1.000000000000000000 ) ) ;
#13280 = VERTEX_POINT ( 'NONE', #17674 ) ;
#13281 = FACE_OUTER_BOUND ( 'NONE', #12760, .T. ) ;
#13282 = ORIENTED_EDGE ( 'NONE', *, *, #8713, .F. ) ;
#13283 = CARTESIAN_POINT ( 'NONE',  ( -16.62983158603122291, -6.888301780572501087, 16.10238750018031695 ) ) ;
#13284 = CARTESIAN_POINT ( 'NONE',  ( -52.00000000000000000, -99.99999999999998579, 0.000000000000000000 ) ) ;
#13285 = VECTOR ( 'NONE', #20317, 1000.000000000000000 ) ;
#13286 = ORIENTED_EDGE ( 'NONE', *, *, #10600, .T. ) ;
#13287 = AXIS2_PLACEMENT_3D ( 'NONE', #1519, #13051, #20785 ) ;
#13288 = DIRECTION ( 'NONE',  ( 0.000000000000000000, -0.7308359642781160348, -0.6825531432186625613 ) ) ;
#13289 = ORIENTED_EDGE ( 'NONE', *, *, #20113, .F. ) ;
#13290 = DIRECTION ( 'NONE',  ( 0.000000000000000000, 0.2697967711570183891, 0.9629172873478009098 ) ) ;
#13291 = PLANE ( 'NONE',  #14155 ) ;
#13292 = AXIS2_PLACEMENT_3D ( 'NONE', #9507, #7920, #376 ) ;
#13293 = ORIENTED_EDGE ( 'NONE', *, *, #7241, .T. ) ;
#13294 = CIRCLE ( 'NONE', #7531, 5.000000000000004441 ) ;
#13295 = CARTESIAN_POINT ( 'NONE',  ( -7.500000000000004441, 9.706494115430842424E-15, -13.76369999999769256 ) ) ;
#13296 = DIRECTION ( 'NONE',  ( -1.000000000000000000, -0.000000000000000000, -0.000000000000000000 ) ) ;
#13297 = CARTESIAN_POINT ( 'NONE',  ( -65.00002539999999840, 0.000000000000000000, 4.000000000000000000 ) ) ;
#13298 = CARTESIAN_POINT ( 'NONE',  ( -9.474249098604513364, -6.330490856366295382, 1.471516000647429268 ) ) ;
#13299 = EDGE_CURVE ( 'NONE', #18355, #16141, #19638, .T. ) ;
#13301 = ORIENTED_EDGE ( 'NONE', *, *, #2945, .F. ) ;
#13300 = AXIS2_PLACEMENT_3D ( 'NONE', #14824, #298, #13227 ) ;
#13302 = DIRECTION ( 'NONE',  ( 0.000000000000000000, 0.000000000000000000, 1.000000000000000000 ) ) ;
#13303 = CIRCLE ( 'NONE', #15955, 2.649999999999987477 ) ;
#13304 = EDGE_CURVE ( 'NONE', #3394, #10440, #1466, .T. ) ;
#13305 = FACE_OUTER_BOUND ( 'NONE', #12517, .T. ) ;
#13306 = AXIS2_PLACEMENT_3D ( 'NONE', #12033, #15213, #20077 ) ;
#13307 = ORIENTED_EDGE ( 'NONE', *, *, #19562, .F. ) ;
#13308 = DIRECTION ( 'NONE',  ( -1.000000000000000000, -0.000000000000000000, -0.000000000000000000 ) ) ;
#13309 = ORIENTED_EDGE ( 'NONE', *, *, #18542, .T. ) ;
#13310 = CARTESIAN_POINT ( 'NONE',  ( 6.888301784570728614, 16.62983158437510056, 12.11636250018031369 ) ) ;
#13311 = CARTESIAN_POINT ( 'NONE',  ( -30.00000000000000000, -164.9999999999999716, 90.00000000000001421 ) ) ;
#13312 = DIRECTION ( 'NONE',  ( 0.000000000000000000, 0.000000000000000000, 1.000000000000000000 ) ) ;
#13313 = AXIS2_PLACEMENT_3D ( 'NONE', #11639, #8146, #16111 ) ;
#13314 = AXIS2_PLACEMENT_3D ( 'NONE', #9537, #17400, #4568 ) ;
#13315 = EDGE_LOOP ( 'NONE', ( #3777, #1637 ) ) ;
#13316 = DIRECTION ( 'NONE',  ( 0.000000000000000000, 0.000000000000000000, 1.000000000000000000 ) ) ;
#13317 = EDGE_LOOP ( 'NONE', ( #6663, #15837, #13883, #18918, #4701, #5226 ) ) ;
#13318 = AXIS2_PLACEMENT_3D ( 'NONE', #12991, #5338, #19444 ) ;
#13319 = CARTESIAN_POINT ( 'NONE',  ( -12.50000000000000533, 0.000000000000000000, 129.0000000000000000 ) ) ;
#13320 = AXIS2_PLACEMENT_3D ( 'NONE', #14773, #18059, #8198 ) ;
#13321 = ORIENTED_EDGE ( 'NONE', *, *, #15191, .F. ) ;
#13322 = DIRECTION ( 'NONE',  ( -0.000000000000000000, -0.000000000000000000, -1.000000000000000000 ) ) ;
#13323 = DIRECTION ( 'NONE',  ( 0.000000000000000000, 0.000000000000000000, 1.000000000000000000 ) ) ;
#13324 = APPLICATION_PROTOCOL_DEFINITION ( 'draft international standard', 'automotive_design', 1998, #3167 ) ;
#13325 = CARTESIAN_POINT ( 'NONE',  ( 1.779017513685136568E-09, 14.79893867758297610, 22.80904191884154741 ) ) ;
#13326 = AXIS2_PLACEMENT_3D ( 'NONE', #13022, #9732, #8133 ) ;
#13327 = ORIENTED_EDGE ( 'NONE', *, *, #3568, .F. ) ;
#13328 = EDGE_CURVE ( 'NONE', #3608, #19557, #10761, .T. ) ;
#13329 = DIRECTION ( 'NONE',  ( -1.000000000000000000, -0.000000000000000000, 0.000000000000000000 ) ) ;
#13330 = ORIENTED_EDGE ( 'NONE', *, *, #19965, .F. ) ;
#13331 = AXIS2_PLACEMENT_3D ( 'NONE', #19620, #16341, #336 ) ;
#13332 = CYLINDRICAL_SURFACE ( 'NONE', #4331, 17.50000000000000355 ) ;
#13333 = CIRCLE ( 'NONE', #9264, 72.00000000007199219 ) ;
#13334 = CARTESIAN_POINT ( 'NONE',  ( -6.888301780572500199, 16.62983158603121936, 18.45863750018030913 ) ) ;
#13335 = FACE_OUTER_BOUND ( 'NONE', #5852, .T. ) ;
#13336 = ADVANCED_FACE ( 'NONE', ( #10107, #11589 ), #9615, .F. ) ;
#13337 = ADVANCED_FACE ( 'NONE', ( #12700 ), #14103, .T. ) ;
#13338 = EDGE_LOOP ( 'NONE', ( #19004, #20710, #2278, #3760, #12812, #5063 ) ) ;
#13339 = DIRECTION ( 'NONE',  ( -1.000000000000000000, 0.000000000000000000, 0.000000000000000000 ) ) ;
#13340 = CARTESIAN_POINT ( 'NONE',  ( 45.76122707727121508, -127.3290820621008947, -85.00000000000000000 ) ) ;
#13341 = AXIS2_PLACEMENT_3D ( 'NONE', #20488, #19008, #15925 ) ;
#13342 = ORIENTED_EDGE ( 'NONE', *, *, #20183, .F. ) ;
#13343 = VECTOR ( 'NONE', #15021, 1000.000000000000000 ) ;
#13344 = DIRECTION ( 'NONE',  ( 0.000000000000000000, 0.000000000000000000, 1.000000000000000000 ) ) ;
#13345 = ORIENTED_EDGE ( 'NONE', *, *, #1087, .T. ) ;
#13346 = CARTESIAN_POINT ( 'NONE',  ( 19.99999999999999645, -64.36139404985985379, 32.27399814043853610 ) ) ;
#13347 = CARTESIAN_POINT ( 'NONE',  ( -12.72792206288790950, -12.72792205982779556, -3.336674999819690068 ) ) ;
#13348 = ORIENTED_EDGE ( 'NONE', *, *, #3009, .F. ) ;
#13349 = ORIENTED_EDGE ( 'NONE', *, *, #13299, .F. ) ;
#13350 = DIRECTION ( 'NONE',  ( -1.000000000000000000, 0.000000000000000000, 0.000000000000000000 ) ) ;
#13351 = EDGE_CURVE ( 'NONE', #11746, #6180, #1636, .T. ) ;
#13352 = AXIS2_PLACEMENT_3D ( 'NONE', #13284, #8493, #1844 ) ;
#13353 = DIRECTION ( 'NONE',  ( 0.000000000000000000, 0.000000000000000000, -1.000000000000000000 ) ) ;
#13354 = DIRECTION ( 'NONE',  ( 0.000000000000000000, 0.000000000000000000, -1.000000000000000000 ) ) ;
#13355 = FACE_OUTER_BOUND ( 'NONE', #13549, .T. ) ;
#13356 = DIRECTION ( 'NONE',  ( 0.000000000000000000, 0.000000000000000000, 1.000000000000000000 ) ) ;
#13357 = CARTESIAN_POINT ( 'NONE',  ( -1.491842756249033064, -7.499999999820668783, 18.71448125018031661 ) ) ;
#13358 = VECTOR ( 'NONE', #5207, 1000.000000000000000 ) ;
#13359 = CARTESIAN_POINT ( 'NONE',  ( 4.276731815070940357, 10.32494394706615815, -11.24729725028680782 ) ) ;
#13360 = CARTESIAN_POINT ( 'NONE',  ( -3.345653888883663996, 2.687187980154699840, -5.460849780464863024 ) ) ;
#13361 = CARTESIAN_POINT ( 'NONE',  ( 19.99999999999999645, 48.70996102988739551, -42.79495875147724604 ) ) ;
#13362 = EDGE_CURVE ( 'NONE', #16164, #10418, #8025, .T. ) ;
#13363 = CIRCLE ( 'NONE', #11325, 65.24900000006526568 ) ;
#13364 = VERTEX_POINT ( 'NONE', #3144 ) ;
#13365 = CARTESIAN_POINT ( 'NONE',  ( 24.99999999999999645, -99.99999999999998579, -54.09999999999999432 ) ) ;
#13366 = EDGE_CURVE ( 'NONE', #18697, #15776, #5325, .T. ) ;
#13367 = CARTESIAN_POINT ( 'NONE',  ( 2.163825119083639534E-09, 18.00000000000000000, 2.102300000180311823 ) ) ;
#13368 = FACE_OUTER_BOUND ( 'NONE', #1712, .T. ) ;
#13369 = ORIENTED_EDGE ( 'NONE', *, *, #3142, .T. ) ;
#13370 = CYLINDRICAL_SURFACE ( 'NONE', #807, 2.099999999999997868 ) ;
#13371 = EDGE_LOOP ( 'NONE', ( #4216, #5578, #11101, #8743 ) ) ;
#13372 = DIRECTION ( 'NONE',  ( 0.000000000000000000, 0.000000000000000000, -1.000000000000000000 ) ) ;
#13373 = FACE_OUTER_BOUND ( 'NONE', #4465, .T. ) ;
#13374 = EDGE_CURVE ( 'NONE', #18597, #3064, #16563, .T. ) ;
#13375 = ORIENTED_EDGE ( 'NONE', *, *, #296, .T. ) ;
#13376 = EDGE_CURVE ( 'NONE', #17173, #5499, #8500, .T. ) ;
#13377 = ORIENTED_EDGE ( 'NONE', *, *, #11371, .T. ) ;
#13378 = PRESENTATION_LAYER_ASSIGNMENT (  '', '', ( #7959 ) ) ;
#13379 = DIRECTION ( 'NONE',  ( 0.000000000000000000, -0.000000000000000000, 1.000000000000000000 ) ) ;
#13380 = PRODUCT_DEFINITION ( 'UNKNOWN', '', #18118, #20001 ) ;
#13381 = CARTESIAN_POINT ( 'NONE',  ( -26.35784117651625280, 26.35784117651607872, -120.0000000000000142 ) ) ;
#13382 = CIRCLE ( 'NONE', #5927, 0.06721999999999977993 ) ;
#13383 = DIRECTION ( 'NONE',  ( -0.000000000000000000, -0.000000000000000000, 1.000000000000000000 ) ) ;
#13384 = EDGE_CURVE ( 'NONE', #18188, #1717, #10421, .T. ) ;
#13385 = EDGE_CURVE ( 'NONE', #13609, #2919, #16795, .T. ) ;
#13386 = CARTESIAN_POINT ( 'NONE',  ( -2.870125743571140919, -6.929096493489624642, 3.319112500180312786 ) ) ;
#13387 = CARTESIAN_POINT ( 'NONE',  ( 39.25023869350728489, -121.8876331835572415, -86.53734499821167958 ) ) ;
#13388 = CARTESIAN_POINT ( 'NONE',  ( 0.000000000000000000, -54.08351995568681048, -35.76369202524558233 ) ) ;
#13389 = AXIS2_PLACEMENT_3D ( 'NONE', #19665, #17791, #180 ) ;
#13390 = LINE ( 'NONE', #13808, #6451 ) ;
#13391 = CARTESIAN_POINT ( 'NONE',  ( 2.500000000000000000, 3.004629197474318851E-15, 2.042000000000000259 ) ) ;
#13392 = ORIENTED_EDGE ( 'NONE', *, *, #4964, .F. ) ;
#13393 = DIRECTION ( 'NONE',  ( -1.000000000000000000, -0.000000000000000000, -0.000000000000000000 ) ) ;
#13394 = EDGE_CURVE ( 'NONE', #10678, #11409, #17873, .T. ) ;
#13395 = EDGE_LOOP ( 'NONE', ( #10084, #9833, #10710, #4899 ) ) ;
#13396 = CARTESIAN_POINT ( 'NONE',  ( 19.99999999999999645, 0.000000000000000000, 0.000000000000000000 ) ) ;
#13397 = CARTESIAN_POINT ( 'NONE',  ( -21.25952603694473808, -3.390848217253790597, 82.75718265314236533 ) ) ;
#13398 = ORIENTED_EDGE ( 'NONE', *, *, #166, .T. ) ;
#13399 = CARTESIAN_POINT ( 'NONE',  ( -52.00000000000000000, -39.99999999999999289, 0.000000000000000000 ) ) ;
#13400 = ORIENTED_EDGE ( 'NONE', *, *, #16550, .F. ) ;
#13401 = EDGE_CURVE ( 'NONE', #12057, #15454, #1363, .T. ) ;
#13402 = DIRECTION ( 'NONE',  ( 0.000000000000000000, 0.000000000000000000, 1.000000000000000000 ) ) ;
#13403 = CARTESIAN_POINT ( 'NONE',  ( 0.000000000000000000, 0.000000000000000000, 0.000000000000000000 ) ) ;
#13404 = EDGE_LOOP ( 'NONE', ( #11495, #15388, #3828, #8177 ) ) ;
#13405 = CARTESIAN_POINT ( 'NONE',  ( 4.248408730893246776, 6.358192987158592047, -10.52385624981969414 ) ) ;
#13406 = CARTESIAN_POINT ( 'NONE',  ( -12.72792206288790950, -12.72792205982779556, -12.76167499981969300 ) ) ;
#13407 = SURFACE_STYLE_FILL_AREA ( #1478 ) ;
#13408 = CIRCLE ( 'NONE', #8636, 27.60000000002759890 ) ;
#13409 = DIRECTION ( 'NONE',  ( -1.000000000000000000, -0.000000000000000000, 0.000000000000000000 ) ) ;
#13410 = CARTESIAN_POINT ( 'NONE',  ( -11.17563879704982988, 2.222972771497744748, 2.649641000647427802 ) ) ;
#13411 = ORIENTED_EDGE ( 'NONE', *, *, #15161, .T. ) ;
#13412 = EDGE_CURVE ( 'NONE', #11338, #3544, #20569, .T. ) ;
#13413 = VECTOR ( 'NONE', #17828, 1000.000000000000000 ) ;
#13414 =( NAMED_UNIT ( * ) SI_UNIT ( $, .STERADIAN. ) SOLID_ANGLE_UNIT ( ) );
#13415 = DIRECTION ( 'NONE',  ( -1.000000000000000000, -0.000000000000000000, -0.000000000000000000 ) ) ;
#13416 = VERTEX_POINT ( 'NONE', #6917 ) ;
#13417 = CARTESIAN_POINT ( 'NONE',  ( -21.39626923676110337, -2.341574137301850822, -83.84978971573227113 ) ) ;
#13418 = ORIENTED_EDGE ( 'NONE', *, *, #17151, .F. ) ;
#13419 = CARTESIAN_POINT ( 'NONE',  ( -17.99999999956958519, 3.580422614997674113, 0.04058125018031183417 ) ) ;
#13420 = DIRECTION ( 'NONE',  ( -1.000000000000000000, 0.000000000000000000, -0.000000000000000000 ) ) ;
#13421 = DIRECTION ( 'NONE',  ( 1.000000000000000000, 0.000000000000000000, 0.000000000000000000 ) ) ;
#13422 = ORIENTED_EDGE ( 'NONE', *, *, #9057, .F. ) ;
#13423 = FACE_BOUND ( 'NONE', #8380, .T. ) ;
#13424 = ORIENTED_EDGE ( 'NONE', *, *, #9374, .T. ) ;
#13425 = CYLINDRICAL_SURFACE ( 'NONE', #446, 21.50000000000000000 ) ;
#13426 = CIRCLE ( 'NONE', #13091, 4.000000000000000000 ) ;
#13427 = AXIS2_PLACEMENT_3D ( 'NONE', #3242, #13421, #16274 ) ;
#13428 = EDGE_CURVE ( 'NONE', #8227, #20014, #19501, .T. ) ;
#13429 = CIRCLE ( 'NONE', #4281, 2.649999999999993694 ) ;
#13430 = EDGE_LOOP ( 'NONE', ( #3349, #16267, #7155, #2660 ) ) ;
#13431 = CARTESIAN_POINT ( 'NONE',  ( 4.000000000000003553, 2.309401076758524685, -5.242734410091827613 ) ) ;
#13432 = CIRCLE ( 'NONE', #575, 27.60000000002760245 ) ;
#13433 = LINE ( 'NONE', #16699, #2799 ) ;
#13434 = CARTESIAN_POINT ( 'NONE',  ( 10.46442989454075700, 10.46442989202484419, 14.56216691884154812 ) ) ;
#13435 = ORIENTED_EDGE ( 'NONE', *, *, #13908, .F. ) ;
#13436 = AXIS2_PLACEMENT_3D ( 'NONE', #2415, #8876, #7285 ) ;
#13437 = VECTOR ( 'NONE', #9418, 1000.000000000000000 ) ;
#13438 = CARTESIAN_POINT ( 'NONE',  ( -12.50000000000000533, 0.000000000000000000, 129.0000000000000000 ) ) ;
#13439 = ORIENTED_EDGE ( 'NONE', *, *, #3243, .T. ) ;
#13440 = CARTESIAN_POINT ( 'NONE',  ( 0.000000000000000000, 0.000000000000000000, 126.0000000000000000 ) ) ;
#13441 = CARTESIAN_POINT ( 'NONE',  ( 12.72792206288790773, 12.72792205982779912, 20.22582500018031482 ) ) ;
#13442 = COLOUR_RGB ( '', 0.66274510, 0.83137255, 0.94901961) ;
#13443 = DIRECTION ( 'NONE',  ( 0.000000000000000000, 0.000000000000000000, -1.000000000000000000 ) ) ;
#13444 = ORIENTED_EDGE ( 'NONE', *, *, #11654, .F. ) ;
#13445 = FACE_OUTER_BOUND ( 'NONE', #7014, .T. ) ;
#13446 = DIRECTION ( 'NONE',  ( 0.000000000000000000, 1.000000000000000000, -1.287488025362403787E-15 ) ) ;
#13447 = AXIS2_PLACEMENT_3D ( 'NONE', #1289, #18768, #4236 ) ;
#13448 = VERTEX_POINT ( 'NONE', #7807 ) ;
#13449 = LINE ( 'NONE', #11636, #12272 ) ;
#13450 = EDGE_LOOP ( 'NONE', ( #2848, #16536, #1148, #11244 ) ) ;
#13451 = CARTESIAN_POINT ( 'NONE',  ( 6.250000000000054179, 10.82531754730546147, 126.0000000000000000 ) ) ;
#13452 = CARTESIAN_POINT ( 'NONE',  ( -10.19618095047497874, 15.25966317163202746, -0.6858937498196888694 ) ) ;
#13453 = ADVANCED_FACE ( 'NONE', ( #20940, #13189, #14877, #6805 ), #13291, .T. ) ;
#13454 = ORIENTED_EDGE ( 'NONE', *, *, #7266, .F. ) ;
#13455 = ORIENTED_EDGE ( 'NONE', *, *, #13526, .T. ) ;
#13456 = FACE_OUTER_BOUND ( 'NONE', #9084, .T. ) ;
#13457 = VECTOR ( 'NONE', #5959, 1000.000000000000000 ) ;
#13458 = CARTESIAN_POINT ( 'NONE',  ( 19.99999999999999645, 59.31169354540738681, 27.19476070466876649 ) ) ;
#13459 = DIRECTION ( 'NONE',  ( 0.000000000000000000, 0.000000000000000000, 1.000000000000000000 ) ) ;
#13460 = SHAPE_REPRESENTATION_RELATIONSHIP ( 'NONE' , 'NONE' ,  #11016, #16501 ) ;
#13461 = CARTESIAN_POINT ( 'NONE',  ( -4.248408729364580694, 6.358192988180020322, -15.45114374981968552 ) ) ;
#13462 = UNCERTAINTY_MEASURE_WITH_UNIT (LENGTH_MEASURE( 1.000000000000000082E-05 ), #3645, 'distance_accuracy_value', 'NONE');
#13463 = DIRECTION ( 'NONE',  ( -1.551631016079434906E-16, 1.000000000000000000, 0.000000000000000000 ) ) ;
#13464 = CARTESIAN_POINT ( 'NONE',  ( -6.358192988180021210, -4.248408729364580694, 1.042606250180315497 ) ) ;
#13465 = VECTOR ( 'NONE', #18062, 999.9999999999998863 ) ;
#13466 = CARTESIAN_POINT ( 'NONE',  ( -2.222972768810836275, 11.17563879758427525, -12.13089100028680534 ) ) ;
#13467 = AXIS2_PLACEMENT_3D ( 'NONE', #7148, #20080, #5559 ) ;
#13468 = CARTESIAN_POINT ( 'NONE',  ( 19.99999999999999645, 0.000000000000000000, 0.000000000000000000 ) ) ;
#13469 = CARTESIAN_POINT ( 'NONE',  ( -15.15000000000000036, 3.245314017740477087E-16, 43.00000000000000000 ) ) ;
#13470 = VECTOR ( 'NONE', #16098, 1000.000000000000000 ) ;
#13471 = ORIENTED_EDGE ( 'NONE', *, *, #17627, .F. ) ;
#13472 = CARTESIAN_POINT ( 'NONE',  ( 52.00000000000000000, -99.99999999999998579, 5.000000000000000000 ) ) ;
#13473 = CARTESIAN_POINT ( 'NONE',  ( 3.580422614997668340, 17.99999999956958519, -7.028168749819689864 ) ) ;
#13474 = DIRECTION ( 'NONE',  ( 1.000000000000000000, 0.000000000000000000, -0.000000000000000000 ) ) ;
#13475 = VERTEX_POINT ( 'NONE', #996 ) ;
#13476 = CARTESIAN_POINT ( 'NONE',  ( 50.00000000000000000, -164.9999999999999716, -90.00000000000001421 ) ) ;
#13477 = ORIENTED_EDGE ( 'NONE', *, *, #10804, .F. ) ;
#13478 = DIRECTION ( 'NONE',  ( -1.000000000000000000, -0.000000000000000000, 0.000000000000000000 ) ) ;
#13479 = CYLINDRICAL_SURFACE ( 'NONE', #14777, 65.24900000006525147 ) ;
#13480 = ORIENTED_EDGE ( 'NONE', *, *, #4017, .F. ) ;
#13481 = ORIENTED_EDGE ( 'NONE', *, *, #803, .T. ) ;
#13482 = LINE ( 'NONE', #20246, #3583 ) ;
#13483 = CARTESIAN_POINT ( 'NONE',  ( 48.35276434571220250, -3.649167310370807105, -90.00000000000000000 ) ) ;
#13484 = EDGE_CURVE ( 'NONE', #18682, #2149, #5855, .T. ) ;
#13485 = EDGE_CURVE ( 'NONE', #15210, #18587, #13133, .T. ) ;
#13486 = FACE_OUTER_BOUND ( 'NONE', #12230, .T. ) ;
#13487 = CARTESIAN_POINT ( 'NONE',  ( 6.358192988180013216, 4.248408729364577141, -9.934793749819688102 ) ) ;
#13488 = CARTESIAN_POINT ( 'NONE',  ( 19.99999999999999645, -36.54710069451090959, 54.05313526368099986 ) ) ;
#13489 = ADVANCED_FACE ( 'NONE', ( #5640 ), #10317, .T. ) ;
#13490 = DIRECTION ( 'NONE',  ( -1.000000000000000000, 0.000000000000000000, 0.000000000000000000 ) ) ;
#13491 = FACE_OUTER_BOUND ( 'NONE', #6688, .T. ) ;
#13492 = DIRECTION ( 'NONE',  ( 0.000000000000000000, -0.2697967711570314897, 0.9629172873477973571 ) ) ;
#13493 = ORIENTED_EDGE ( 'NONE', *, *, #6048, .F. ) ;
#13494 = LINE ( 'NONE', #19936, #2097 ) ;
#13495 = VERTEX_POINT ( 'NONE', #2467 ) ;
#13496 = CARTESIAN_POINT ( 'NONE',  ( 17.99999999956958163, -3.580422614997676334, 2.848481250180313840 ) ) ;
#13497 = CARTESIAN_POINT ( 'NONE',  ( -3.872723063507635732, -21.16211945945223505, 70.72147569179593063 ) ) ;
#13498 = VERTEX_POINT ( 'NONE', #10426 ) ;
#13499 = LINE ( 'NONE', #663, #8567 ) ;
#13500 = EDGE_LOOP ( 'NONE', ( #8125, #6038 ) ) ;
#13501 = DIRECTION ( 'NONE',  ( -0.4999999999999918954, 0.8660254037844433705, 0.000000000000000000 ) ) ;
#13502 = DIRECTION ( 'NONE',  ( 0.000000000000000000, 0.000000000000000000, 1.000000000000000000 ) ) ;
#13503 = ORIENTED_EDGE ( 'NONE', *, *, #1348, .F. ) ;
#13504 = ADVANCED_FACE ( 'NONE', ( #2261 ), #20370, .F. ) ;
#13505 = FACE_OUTER_BOUND ( 'NONE', #14774, .T. ) ;
#13506 = CARTESIAN_POINT ( 'NONE',  ( -6.888301784570736608, -16.62983158437509346, -13.35073749981969371 ) ) ;
#13507 = CARTESIAN_POINT ( 'NONE',  ( 0.2500000000000002220, 0.000000000000000000, 0.000000000000000000 ) ) ;
#13508 = ADVANCED_FACE ( 'NONE', ( #16981 ), #19944, .T. ) ;
#13509 = EDGE_CURVE ( 'NONE', #6065, #15909, #3255, .T. ) ;
#13510 = FACE_OUTER_BOUND ( 'NONE', #18029, .T. ) ;
#13511 = CIRCLE ( 'NONE', #19255, 2.649999999999987477 ) ;
#13512 = CARTESIAN_POINT ( 'NONE',  ( 1.343451552857795926E-09, 11.17563879731705789, 4.711359750647427624 ) ) ;
#13513 = ORIENTED_EDGE ( 'NONE', *, *, #14886, .F. ) ;
#13514 = CARTESIAN_POINT ( 'NONE',  ( 50.00000000000000000, -42.57363661491096707, -121.3828884801879155 ) ) ;
#13515 = VERTEX_POINT ( 'NONE', #12218 ) ;
#13516 = CARTESIAN_POINT ( 'NONE',  ( -9.249412617561571182, -19.41235462500714348, -71.49717528132289601 ) ) ;
#13517 = ORIENTED_EDGE ( 'NONE', *, *, #15582, .T. ) ;
#13518 = CARTESIAN_POINT ( 'NONE',  ( 3.580422610670020322, -18.00000000043041126, -2.904731249819686667 ) ) ;
#13519 = DIRECTION ( 'NONE',  ( 1.000000000000000000, 0.000000000000000000, 0.000000000000000000 ) ) ;
#13520 = DIRECTION ( 'NONE',  ( 0.000000000000000000, 0.000000000000000000, 1.000000000000000000 ) ) ;
#13521 = ORIENTED_EDGE ( 'NONE', *, *, #7940, .F. ) ;
#13522 = ORIENTED_EDGE ( 'NONE', *, *, #12265, .F. ) ;
#13523 = DIRECTION ( 'NONE',  ( 0.000000000000000000, 0.8660254037844380415, -0.5000000000000011102 ) ) ;
#13524 = ORIENTED_EDGE ( 'NONE', *, *, #6652, .F. ) ;
#13525 = DIRECTION ( 'NONE',  ( -1.000000000000000000, 0.000000000000000000, 0.000000000000000000 ) ) ;
#13526 = EDGE_CURVE ( 'NONE', #9439, #880, #3728, .T. ) ;
#13527 = EDGE_LOOP ( 'NONE', ( #3537, #18794, #5252, #4371 ) ) ;
#13528 = DIRECTION ( 'NONE',  ( -0.000000000000000000, -0.000000000000000000, 1.000000000000000000 ) ) ;
#13529 = ADVANCED_FACE ( 'NONE', ( #4046 ), #11894, .T. ) ;
#13530 = DIRECTION ( 'NONE',  ( -1.000000000000000000, -0.000000000000000000, -0.000000000000000000 ) ) ;
#13531 = CONTEXT_DEPENDENT_SHAPE_REPRESENTATION ( #1300, #2392 ) ;
#13532 = CARTESIAN_POINT ( 'NONE',  ( 15.25966316918061771, -10.19618095414378800, -22.93285624981969306 ) ) ;
#13533 = ORIENTED_EDGE ( 'NONE', *, *, #14449, .F. ) ;
#13534 = FACE_OUTER_BOUND ( 'NONE', #3541, .T. ) ;
#13535 = LINE ( 'NONE', #7375, #7088 ) ;
#13536 = AXIS2_PLACEMENT_3D ( 'NONE', #1541, #17437, #3013 ) ;
#13537 = CARTESIAN_POINT ( 'NONE',  ( 8.382925368423265411, -12.54593441764187034, -26.10513566848092992 ) ) ;
#13538 = EDGE_CURVE ( 'NONE', #15733, #18615, #3833, .T. ) ;
#13539 = CARTESIAN_POINT ( 'NONE',  ( -10.00000000000000000, 0.000000000000000000, 0.000000000000000000 ) ) ;
#13540 = ORIENTED_EDGE ( 'NONE', *, *, #1611, .T. ) ;
#13541 = CARTESIAN_POINT ( 'NONE',  ( 33.05360093408142319, -115.6303066365226471, 81.70693292403575470 ) ) ;
#13542 = CARTESIAN_POINT ( 'NONE',  ( 45.06005321672401465, -126.4314683844613683, -83.99502465749384328 ) ) ;
#13543 = ORIENTED_EDGE ( 'NONE', *, *, #8842, .F. ) ;
#13544 = DIRECTION ( 'NONE',  ( 0.000000000000000000, 0.000000000000000000, -1.000000000000000000 ) ) ;
#13545 = ORIENTED_EDGE ( 'NONE', *, *, #20724, .F. ) ;
#13546 = DIRECTION ( 'NONE',  ( -1.000000000000000000, -0.000000000000000000, 0.000000000000000000 ) ) ;
#13547 = CARTESIAN_POINT ( 'NONE',  ( 16.62983158603121936, 6.888301780572501976, 1.964887500180308777 ) ) ;
#13548 = ORIENTED_EDGE ( 'NONE', *, *, #18009, .F. ) ;
#13549 = EDGE_LOOP ( 'NONE', ( #6650, #18883, #1293, #6748 ) ) ;
#13550 = DIRECTION ( 'NONE',  ( -1.000000000000000000, 0.000000000000000000, 0.000000000000000000 ) ) ;
#13551 = CIRCLE ( 'NONE', #3069, 27.60000000002759890 ) ;
#13552 = CARTESIAN_POINT ( 'NONE',  ( 52.50000000000000000, -30.00000000000000000, 0.000000000000000000 ) ) ;
#13553 = CARTESIAN_POINT ( 'NONE',  ( -30.00000000000000000, -40.00000000000000000, -120.0000000000000142 ) ) ;
#13554 = CARTESIAN_POINT ( 'NONE',  ( 2.870125743571140475, 6.929096493489632635, -13.97848749981969085 ) ) ;
#13555 = DIRECTION ( 'NONE',  ( -1.000000000000000000, -0.000000000000000000, -0.000000000000000000 ) ) ;
#13556 = CARTESIAN_POINT ( 'NONE',  ( -1.491842756249033064, -7.499999999820668783, -0.1355187498196866458 ) ) ;
#13557 = AXIS2_PLACEMENT_3D ( 'NONE', #20031, #11574, #10411 ) ;
#13558 = EDGE_CURVE ( 'NONE', #12428, #8862, #12416, .T. ) ;
#13559 = CARTESIAN_POINT ( 'NONE',  ( -6.330490856366290053, 9.474249098604506258, -22.14495350028680676 ) ) ;
#13560 = PRODUCT_DEFINITION_SHAPE ( 'NONE', 'NONE',  #20968 ) ;
#13561 = EDGE_CURVE ( 'NONE', #8326, #8346, #17153, .T. ) ;
#13562 = CARTESIAN_POINT ( 'NONE',  ( 5.200000000000002842, 0.000000000000000000, 0.000000000000000000 ) ) ;
#13563 = EDGE_LOOP ( 'NONE', ( #11946, #8001, #16657, #10748 ) ) ;
#13564 = CARTESIAN_POINT ( 'NONE',  ( 17.50000000000000355, 0.000000000000000000, 129.0000000000000000 ) ) ;
#13565 = CIRCLE ( 'NONE', #702, 72.00000000007199219 ) ;
#13566 = CARTESIAN_POINT ( 'NONE',  ( 15.25966316918061416, -10.19618095414378622, -4.082856249819688088 ) ) ;
#13567 = DIRECTION ( 'NONE',  ( 0.000000000000000000, 0.000000000000000000, -1.000000000000000000 ) ) ;
#13568 = EDGE_LOOP ( 'NONE', ( #17281, #11870, #9000, #9093 ) ) ;
#13569 = DIRECTION ( 'NONE',  ( 0.000000000000000000, 0.4999999999999993339, -0.8660254037844390407 ) ) ;
#13570 = ORIENTED_EDGE ( 'NONE', *, *, #3908, .T. ) ;
#13571 = CARTESIAN_POINT ( 'NONE',  ( 19.99999999999999645, -23.08379033237309841, -61.02926039941459635 ) ) ;
#13572 = CARTESIAN_POINT ( 'NONE',  ( 41.63608460325703220, -13.17366712949431218, -74.81088764122226564 ) ) ;
#13573 = ORIENTED_EDGE ( 'NONE', *, *, #10403, .F. ) ;
#13574 = VECTOR ( 'NONE', #665, 1000.000000000000000 ) ;
#13575 = ORIENTED_EDGE ( 'NONE', *, *, #6223, .T. ) ;
#13576 = CYLINDRICAL_SURFACE ( 'NONE', #8324, 39.99999999999999289 ) ;
#13577 = CARTESIAN_POINT ( 'NONE',  ( 19.99999999999999645, -49.77519642624036322, 42.18840861821767163 ) ) ;
#13578 = FACE_OUTER_BOUND ( 'NONE', #218, .T. ) ;
#13579 = AXIS2_PLACEMENT_3D ( 'NONE', #5133, #8318, #18080 ) ;
#13580 = CARTESIAN_POINT ( 'NONE',  ( 7.500000000179339210, 1.491842754445841690, 0.07926875018031064035 ) ) ;
#13581 = DIRECTION ( 'NONE',  ( 1.000000000000000000, -0.000000000000000000, -0.000000000000000000 ) ) ;
#13582 = AXIS2_PLACEMENT_3D ( 'NONE', #18135, #1823, #6684 ) ;
#13583 = SURFACE_SIDE_STYLE ('',( #10304 ) ) ;
#13584 = CARTESIAN_POINT ( 'NONE',  ( 2.500000000000000000, 1.178949249685213863, -2.042000000000001148 ) ) ;
#13585 = LINE ( 'NONE', #20033, #17403 ) ;
#13586 = ORIENTED_EDGE ( 'NONE', *, *, #13601, .F. ) ;
#13587 = CARTESIAN_POINT ( 'NONE',  ( 5.303300859536635770, 5.303300858261589923, 5.460575000180316607 ) ) ;
#13588 = ORIENTED_EDGE ( 'NONE', *, *, #11023, .T. ) ;
#13589 = CARTESIAN_POINT ( 'NONE',  ( -12.72792206288791128, -12.72792205982779912, -3.336674999819686516 ) ) ;
#13590 = CARTESIAN_POINT ( 'NONE',  ( 11.44271251907791154, -18.21718295280816236, 72.06823551977507236 ) ) ;
#13591 = APPLICATION_CONTEXT ( 'automotive_design' ) ;
#13592 = VERTEX_POINT ( 'NONE', #16887 ) ;
#13593 = EDGE_CURVE ( 'NONE', #9981, #11587, #5290, .T. ) ;
#13594 = FACE_OUTER_BOUND ( 'NONE', #14831, .T. ) ;
#13595 = ORIENTED_EDGE ( 'NONE', *, *, #9254, .T. ) ;
#13596 = DIRECTION ( 'NONE',  ( -1.000000000000000000, -0.000000000000000000, 0.000000000000000000 ) ) ;
#13597 = DIRECTION ( 'NONE',  ( -1.000000000000000000, 0.000000000000000000, 0.000000000000000000 ) ) ;
#13598 = VERTEX_POINT ( 'NONE', #7023 ) ;
#13599 = CYLINDRICAL_SURFACE ( 'NONE', #8996, 65.24900000006525147 ) ;
#13600 = CIRCLE ( 'NONE', #15976, 75.00000000000001421 ) ;
#13601 = EDGE_CURVE ( 'NONE', #10695, #9587, #13761, .T. ) ;
#13602 = CARTESIAN_POINT ( 'NONE',  ( -24.99999999999999289, -160.0000000000000000, 0.000000000000000000 ) ) ;
#13603 = CARTESIAN_POINT ( 'NONE',  ( 15.25966317163202568, 10.19618095047498230, -17.17964374981969655 ) ) ;
#13604 = CARTESIAN_POINT ( 'NONE',  ( 0.000000000000000000, 64.36139404985965484, 32.27399814043899084 ) ) ;
#13605 = EDGE_CURVE ( 'NONE', #3634, #9449, #15453, .T. ) ;
#13606 = CARTESIAN_POINT ( 'NONE',  ( 19.99999999999999645, -35.35772184876915958, 54.34979580218180928 ) ) ;
#13607 = PRESENTATION_LAYER_ASSIGNMENT (  '', '', ( #9209 ) ) ;
#13608 = CARTESIAN_POINT ( 'NONE',  ( -1.343452921478824119E-09, -11.17563879731705789, -0.001140249352573480474 ) ) ;
#13609 = VERTEX_POINT ( 'NONE', #13821 ) ;
#13610 = DIRECTION ( 'NONE',  ( -1.000000000000000000, 0.000000000000000000, 0.000000000000000000 ) ) ;
#13611 = FACE_OUTER_BOUND ( 'NONE', #3883, .T. ) ;
#13612 = ORIENTED_EDGE ( 'NONE', *, *, #12046, .T. ) ;
#13613 = CIRCLE ( 'NONE', #16999, 5.000000000000000888 ) ;
#13614 = CARTESIAN_POINT ( 'NONE',  ( -19.43057967899846616, -9.208910241125160212, -77.65734690581830080 ) ) ;
#13615 = ORIENTED_EDGE ( 'NONE', *, *, #8721, .F. ) ;
#13616 = VECTOR ( 'NONE', #393, 1000.000000000000000 ) ;
#13617 = CARTESIAN_POINT ( 'NONE',  ( 6.888301780572507305, -16.62983158603121936, 6.225737500180312800 ) ) ;
#13618 = DIRECTION ( 'NONE',  ( 0.000000000000000000, 0.000000000000000000, 1.000000000000000000 ) ) ;
#13619 = CARTESIAN_POINT ( 'NONE',  ( 50.00000000000000000, -139.6410161513775563, 90.00000000000001421 ) ) ;
#13620 = ORIENTED_EDGE ( 'NONE', *, *, #17288, .T. ) ;
#13621 = EDGE_CURVE ( 'NONE', #19670, #5814, #18585, .T. ) ;
#13622 = LINE ( 'NONE', #13840, #11272 ) ;
#13623 = ORIENTED_EDGE ( 'NONE', *, *, #15828, .F. ) ;
#13624 = DIRECTION ( 'NONE',  ( 0.000000000000000000, 0.000000000000000000, -1.000000000000000000 ) ) ;
#13625 = EDGE_CURVE ( 'NONE', #10361, #9436, #6672, .T. ) ;
#13626 = VERTEX_POINT ( 'NONE', #20482 ) ;
#13627 = CARTESIAN_POINT ( 'NONE',  ( 30.00000000000000000, -85.00000000000000000, -1.040949779275250179E-14 ) ) ;
#13628 = EDGE_CURVE ( 'NONE', #10742, #9288, #1908, .T. ) ;
#13629 = ORIENTED_EDGE ( 'NONE', *, *, #9590, .T. ) ;
#13630 = FACE_OUTER_BOUND ( 'NONE', #16361, .T. ) ;
#13631 = AXIS2_PLACEMENT_3D ( 'NONE', #9421, #7929, #15876 ) ;
#13632 = CIRCLE ( 'NONE', #16009, 17.50000000000000355 ) ;
#13633 = CARTESIAN_POINT ( 'NONE',  ( 30.00000000000001066, 39.99999999999998579, -130.0000000000000000 ) ) ;
#13634 = ITEM_DEFINED_TRANSFORMATION ( 'NONE', 'NONE', #2920,  #12461 ) ;
#13635 = CARTESIAN_POINT ( 'NONE',  ( -10.46442989202484242, 10.46442989454075700, 21.63091691884155310 ) ) ;
#13636 = EDGE_LOOP ( 'NONE', ( #11362, #6321, #6817, #19466 ) ) ;
#13637 = DIRECTION ( 'NONE',  ( 0.000000000000000000, 0.7308359642781252496, -0.6825531432186529024 ) ) ;
#13638 = VECTOR ( 'NONE', #12995, 1000.000000000000000 ) ;
#13639 = EDGE_CURVE ( 'NONE', #4610, #18559, #12437, .T. ) ;
#13640 = CARTESIAN_POINT ( 'NONE',  ( -17.73632026622077618, -12.15589442372808548, 81.69840364569164137 ) ) ;
#13641 = EDGE_CURVE ( 'NONE', #3544, #5249, #13432, .T. ) ;
#13642 = CARTESIAN_POINT ( 'NONE',  ( -14.79893867793683349, -2.943691925285398359, -23.15982316848093348 ) ) ;
#13643 = DIRECTION ( 'NONE',  ( 1.000000000000000000, -0.000000000000000000, -0.000000000000000000 ) ) ;
#13644 = CIRCLE ( 'NONE', #13318, 27.60000000002759890 ) ;
#13645 = CIRCLE ( 'NONE', #17729, 7.500000000000000000 ) ;
#13646 = ORIENTED_EDGE ( 'NONE', *, *, #11064, .T. ) ;
#13647 = EDGE_CURVE ( 'NONE', #17067, #5518, #10840, .T. ) ;
#13648 = CARTESIAN_POINT ( 'NONE',  ( 7.500000000000000888, -2.290195989456150567E-15, 9.798800000002307442 ) ) ;
#13649 = CARTESIAN_POINT ( 'NONE',  ( 41.19307857824662733, -123.0525692265442785, -80.87006134762231113 ) ) ;
#13650 = ORIENTED_EDGE ( 'NONE', *, *, #4617, .F. ) ;
#13651 = CARTESIAN_POINT ( 'NONE',  ( 6.134128071782536828, -22.22025288403098386, -75.71173876110991330 ) ) ;
#13652 = VERTEX_POINT ( 'NONE', #12655 ) ;
#13653 = CARTESIAN_POINT ( 'NONE',  ( 2.500000000000000000, 2.357898499370431722, -2.818925648462311528E-15 ) ) ;
#13654 = CARTESIAN_POINT ( 'NONE',  ( 15.25966316918061239, -10.19618095414378445, 12.86254375018031126 ) ) ;
#13655 = EDGE_LOOP ( 'NONE', ( #5415, #18808, #5322, #7452 ) ) ;
#13656 = CIRCLE ( 'NONE', #7206, 72.00000000007199219 ) ;
#13657 = ORIENTED_EDGE ( 'NONE', *, *, #12871, .T. ) ;
#13658 = CYLINDRICAL_SURFACE ( 'NONE', #12421, 27.60000000002759890 ) ;
#13659 = DIRECTION ( 'NONE',  ( 0.000000000000000000, 0.000000000000000000, 1.000000000000000000 ) ) ;
#13660 = DIRECTION ( 'NONE',  ( 0.000000000000000000, 0.000000000000000000, -1.000000000000000000 ) ) ;
#13661 =( LENGTH_UNIT ( ) NAMED_UNIT ( * ) SI_UNIT ( .MILLI., .METRE. ) );
#13662 = DIRECTION ( 'NONE',  ( 1.000000000000000000, 0.000000000000000000, 0.000000000000000000 ) ) ;
#13663 = AXIS2_PLACEMENT_3D ( 'NONE', #4797, #1643, #17741 ) ;
#13664 = CIRCLE ( 'NONE', #18757, 27.60000000002759890 ) ;
#13665 = PRODUCT_DEFINITION_CONTEXT ( 'detailed design', #4399, 'design' ) ;
#13666 = DIRECTION ( 'NONE',  ( 0.000000000000000000, 1.040834085586084454E-15, -1.000000000000000000 ) ) ;
#13667 = CARTESIAN_POINT ( 'NONE',  ( 1.491842756249030622, 7.499999999820669672, 4.576981250180313765 ) ) ;
#13668 = DIRECTION ( 'NONE',  ( 1.000000000000000000, 0.000000000000000000, 0.000000000000000000 ) ) ;
#13669 = CARTESIAN_POINT ( 'NONE',  ( -11.17563879704981922, 2.222972771497742972, -23.32307850028680463 ) ) ;
#13670 = AXIS2_PLACEMENT_3D ( 'NONE', #7679, #2908, #9378 ) ;
#13671 = DIRECTION ( 'NONE',  ( -1.000000000000000000, -0.000000000000000000, 0.000000000000000000 ) ) ;
#13672 = VECTOR ( 'NONE', #3381, 1000.000000000000000 ) ;
#13673 = ORIENTED_EDGE ( 'NONE', *, *, #18020, .T. ) ;
#13674 = CARTESIAN_POINT ( 'NONE',  ( 3.600000000000060485, 10.82531754730546147, 43.00000000000000000 ) ) ;
#13675 = CARTESIAN_POINT ( 'NONE',  ( 10.19618095414378800, 15.25966316918061416, -6.439106249819689154 ) ) ;
#13676 = CYLINDRICAL_SURFACE ( 'NONE', #14478, 18.00000000000000000 ) ;
#13677 = CIRCLE ( 'NONE', #10596, 72.00000000007199219 ) ;
#13678 = ORIENTED_EDGE ( 'NONE', *, *, #17299, .F. ) ;
#13679 = FACE_OUTER_BOUND ( 'NONE', #7598, .T. ) ;
#13680 = VERTEX_POINT ( 'NONE', #14456 ) ;
#13681 = AXIS2_PLACEMENT_3D ( 'NONE', #1436, #14369, #6296 ) ;
#13682 = FACE_OUTER_BOUND ( 'NONE', #20660, .T. ) ;
#13683 = DIRECTION ( 'NONE',  ( 0.000000000000000000, 0.000000000000000000, 1.000000000000000000 ) ) ;
#13684 = ORIENTED_EDGE ( 'NONE', *, *, #4356, .T. ) ;
#13685 = EDGE_LOOP ( 'NONE', ( #17624, #13570, #19069, #10444 ) ) ;
#13686 = CYLINDRICAL_SURFACE ( 'NONE', #11391, 65.24900000006525147 ) ;
#13687 = EDGE_CURVE ( 'NONE', #12561, #17222, #16810, .T. ) ;
#13688 = CIRCLE ( 'NONE', #4550, 72.00000000007199219 ) ;
#13689 = SHAPE_REPRESENTATION_RELATIONSHIP ( 'NONE' , 'NONE' ,  #8160, #1863 ) ;
#13690 = DIRECTION ( 'NONE',  ( 1.000000000000000000, 0.000000000000000000, -0.000000000000000000 ) ) ;
#13691 = CARTESIAN_POINT ( 'NONE',  ( 19.99999999999999645, 0.000000000000000000, 0.000000000000000000 ) ) ;
#13692 = CIRCLE ( 'NONE', #19781, 200.0000000000000000 ) ;
#13693 = CARTESIAN_POINT ( 'NONE',  ( -7.500000000179339210, -1.491842754445842800, -4.633231249819690589 ) ) ;
#13694 = FACE_OUTER_BOUND ( 'NONE', #15012, .T. ) ;
#13695 = DIRECTION ( 'NONE',  ( -1.000000000000000000, 1.776356839400250465E-15, 0.000000000000000000 ) ) ;
#13696 = DIRECTION ( 'NONE',  ( -1.000000000000000000, -0.000000000000000000, -0.000000000000000000 ) ) ;
#13697 = ORIENTED_EDGE ( 'NONE', *, *, #13123, .F. ) ;
#13698 = CARTESIAN_POINT ( 'NONE',  ( -31.75000000000000000, 0.000000000000000000, 0.000000000000000000 ) ) ;
#13699 = ORIENTED_EDGE ( 'NONE', *, *, #15093, .T. ) ;
#13700 = CARTESIAN_POINT ( 'NONE',  ( 2.163825119083639534E-09, 18.00000000000000000, 9.622700000180314461 ) ) ;
#13701 = DIRECTION ( 'NONE',  ( -1.000000000000000000, -0.000000000000000000, -0.000000000000000000 ) ) ;
#13702 = VERTEX_POINT ( 'NONE', #17210 ) ;
#13703 = DIRECTION ( 'NONE',  ( 0.000000000000000000, 0.000000000000000000, 1.000000000000000000 ) ) ;
#13704 = ORIENTED_EDGE ( 'NONE', *, *, #10802, .T. ) ;
#13705 = CARTESIAN_POINT ( 'NONE',  ( 19.99999999999999645, 64.79224928664392280, -2.456263514197840614 ) ) ;
#13706 = DIRECTION ( 'NONE',  ( 1.000000000000000000, 0.000000000000000000, 0.000000000000000000 ) ) ;
#13707 = B_SPLINE_CURVE_WITH_KNOTS ( 'NONE', 3,
 ( #19050, #15339, #7274, #18623 ),
 .UNSPECIFIED., .F., .F.,
 ( 4, 4 ),
 ( 2.380737582480036903E-07, 0.002336974151641604130 ),
 .UNSPECIFIED. ) ;
#13708 = VERTEX_POINT ( 'NONE', #10945 ) ;
#13709 = DIRECTION ( 'NONE',  ( 0.000000000000000000, 0.000000000000000000, -1.000000000000000000 ) ) ;
#13710 = CIRCLE ( 'NONE', #20465, 11.17999999999999261 ) ;
#13711 = EDGE_CURVE ( 'NONE', #8274, #7282, #15603, .T. ) ;
#13712 = DIRECTION ( 'NONE',  ( -0.000000000000000000, -0.000000000000000000, 1.000000000000000000 ) ) ;
#13713 = CARTESIAN_POINT ( 'NONE',  ( 16.62983158603121936, 6.888301780572501976, -7.460112499819690157 ) ) ;
#13714 = CARTESIAN_POINT ( 'NONE',  ( -4.000000000000000000, 1.557668341133520373, -5.440303434304243346 ) ) ;
#13715 = DIRECTION ( 'NONE',  ( 1.000000000000000000, 1.836909530733573776E-16, 0.000000000000000000 ) ) ;
#13716 = PRODUCT_DEFINITION_FORMATION_WITH_SPECIFIED_SOURCE ( 'ANY', '', #10346, .NOT_KNOWN. ) ;
#13717 = CARTESIAN_POINT ( 'NONE',  ( -6.330490858644140850, -9.474249097082498849, -17.96754649935258286 ) ) ;
#13718 = EDGE_CURVE ( 'NONE', #5869, #20752, #18164, .T. ) ;
#13719 = EDGE_LOOP ( 'NONE', ( #8865, #13573, #19239, #3214 ) ) ;
#13720 = CARTESIAN_POINT ( 'NONE',  ( 19.99999999999999645, 63.85430960833490843, -11.25592921604860663 ) ) ;
#13721 = DIRECTION ( 'NONE',  ( 0.000000000000000000, 0.000000000000000000, 1.000000000000000000 ) ) ;
#13722 = VERTEX_POINT ( 'NONE', #3000 ) ;
#13723 = CARTESIAN_POINT ( 'NONE',  ( 14.60954982181485740, -15.77788197283119409, -73.35099031848521633 ) ) ;
#13724 = CIRCLE ( 'NONE', #11010, 2.649999999999994582 ) ;
#13725 = ORIENTED_EDGE ( 'NONE', *, *, #10184, .T. ) ;
#13726 = CARTESIAN_POINT ( 'NONE',  ( -16.62983158437510056, 6.888301784570729502, 9.760112500180312622 ) ) ;
#13727 = DIRECTION ( 'NONE',  ( -1.000000000000000000, 0.000000000000000000, 0.000000000000000000 ) ) ;
#13728 = CARTESIAN_POINT ( 'NONE',  ( 19.99999999999999645, 24.01204443665271882, -60.22865198596099390 ) ) ;
#13729 = ORIENTED_EDGE ( 'NONE', *, *, #10184, .F. ) ;
#13730 = FACE_BOUND ( 'NONE', #18605, .T. ) ;
#13731 = ORIENTED_EDGE ( 'NONE', *, *, #20511, .F. ) ;
#13732 = CARTESIAN_POINT ( 'NONE',  ( 1.491842756249030399, 7.499999999820669672, 14.00198125018031625 ) ) ;
#13733 = EDGE_LOOP ( 'NONE', ( #3517, #2582, #17525, #14672 ) ) ;
#13734 = DIRECTION ( 'NONE',  ( 0.000000000000000000, 0.000000000000000000, 1.000000000000000000 ) ) ;
#13735 = AXIS2_PLACEMENT_3D ( 'NONE', #7551, #12767, #5962 ) ;
#13736 = DIRECTION ( 'NONE',  ( 0.000000000000000000, 0.000000000000000000, -1.000000000000000000 ) ) ;
#13737 = CARTESIAN_POINT ( 'NONE',  ( 0.000000000000000000, 68.15657073222466522, -23.20952102120210725 ) ) ;
#13738 = ITEM_DEFINED_TRANSFORMATION ( 'NONE', 'NONE', #16398,  #12461 ) ;
#13739 = SHAPE_REPRESENTATION ( 'BR-546', ( #8976, #16398, #6620, #20806, #20161, #7255, #9971, #3535, #18481, #203, #15393, #6255, #18102, #2920, #11039, #1206, #5923, #4909, #15744, #7270, #18452, #15066, #1869, #19142, #170, #13389, #11348 ), #13041 ) ;
#13740 = CARTESIAN_POINT ( 'NONE',  ( 2.943691928843431782, 14.79893867722910628, -5.171426831158459692 ) ) ;
#13741 = EDGE_CURVE ( 'NONE', #5402, #4186, #3592, .T. ) ;
#13742 = ORIENTED_EDGE ( 'NONE', *, *, #11497, .T. ) ;
#13743 = EDGE_CURVE ( 'NONE', #12032, #1037, #4622, .T. ) ;
#13744 = CARTESIAN_POINT ( 'NONE',  ( 9.999999999999998224, -46.17500197033096043, 55.24372537266381755 ) ) ;
#13745 = ORIENTED_EDGE ( 'NONE', *, *, #861, .F. ) ;
#13746 = CARTESIAN_POINT ( 'NONE',  ( 19.99999999999999645, -53.26727847779503833, -48.44168704307685402 ) ) ;
#13747 = CARTESIAN_POINT ( 'NONE',  ( -8.382925371439625906, -12.54593441562639988, -24.33794816848093134 ) ) ;
#13748 = AXIS2_PLACEMENT_3D ( 'NONE', #8698, #15168, #18453 ) ;
#13749 = CARTESIAN_POINT ( 'NONE',  ( 19.99999999999999645, 27.80658314415318699, -66.41380830714092554 ) ) ;
#13750 = ADVANCED_FACE ( 'NONE', ( #15920 ), #2785, .T. ) ;
#13751 = CIRCLE ( 'NONE', #20565, 27.60000000002759890 ) ;
#13752 = CIRCLE ( 'NONE', #10030, 65.24900000006525147 ) ;
#13753 = ORIENTED_EDGE ( 'NONE', *, *, #10644, .T. ) ;
#13754 = CARTESIAN_POINT ( 'NONE',  ( 7.500000000000000000, -9.015933403756339613E-10, -21.63629999981969121 ) ) ;
#13755 = DIRECTION ( 'NONE',  ( 0.000000000000000000, -0.000000000000000000, 1.000000000000000000 ) ) ;
#13756 = ORIENTED_EDGE ( 'NONE', *, *, #13864, .T. ) ;
#13757 = FACE_OUTER_BOUND ( 'NONE', #2234, .T. ) ;
#13758 = ORIENTED_EDGE ( 'NONE', *, *, #5355, .T. ) ;
#13759 = DIRECTION ( 'NONE',  ( 0.000000000000000000, 0.000000000000000000, -1.000000000000000000 ) ) ;
#13760 = CARTESIAN_POINT ( 'NONE',  ( 3.580422614997667896, 17.99999999956958163, 9.917231250180311264 ) ) ;
#13761 = CIRCLE ( 'NONE', #18852, 27.60000000002760245 ) ;
#13762 = VERTEX_POINT ( 'NONE', #7658 ) ;
#13763 = VERTEX_POINT ( 'NONE', #14137 ) ;
#13764 = DIRECTION ( 'NONE',  ( 0.000000000000000000, 0.000000000000000000, -1.000000000000000000 ) ) ;
#13765 = EDGE_CURVE ( 'NONE', #11920, #2829, #3273, .T. ) ;
#13766 = CIRCLE ( 'NONE', #6639, 27.60000000002759890 ) ;
#13767 = DIRECTION ( 'NONE',  ( -1.000000000000000000, 0.000000000000000000, 0.000000000000000000 ) ) ;
#13768 = CIRCLE ( 'NONE', #12067, 27.60000000002760245 ) ;
#13769 = DIRECTION ( 'NONE',  ( 1.000000000000000000, 0.000000000000000000, 0.000000000000000000 ) ) ;
#13770 = DIRECTION ( 'NONE',  ( 0.000000000000000000, 0.000000000000000000, 1.000000000000000000 ) ) ;
#13771 = DIRECTION ( 'NONE',  ( -1.000000000000000000, 0.000000000000000000, 0.000000000000000000 ) ) ;
#13772 = EDGE_CURVE ( 'NONE', #12808, #13364, #1416, .T. ) ;
#13773 = VECTOR ( 'NONE', #2307, 1000.000000000000000 ) ;
#13774 = CIRCLE ( 'NONE', #12319, 17.50000000000000355 ) ;
#13775 = ADVANCED_FACE ( 'NONE', ( #17623 ), #3399, .T. ) ;
#13776 = CARTESIAN_POINT ( 'NONE',  ( 19.99999999999999645, 46.17500197033132281, -55.24372537266349781 ) ) ;
#13777 = CARTESIAN_POINT ( 'NONE',  ( -2.870125741905213079, 6.929096494179683319, 3.693387500180313143 ) ) ;
#13778 = CARTESIAN_POINT ( 'NONE',  ( 7.500000000000007105, -2.290195989506637665E-15, 16.06370000000231357 ) ) ;
#13779 = CARTESIAN_POINT ( 'NONE',  ( -10.32494394809439164, -4.276731812588563386, -24.20667225028680747 ) ) ;
#13780 = EDGE_CURVE ( 'NONE', #3863, #15532, #12958, .T. ) ;
#13781 = AXIS2_PLACEMENT_3D ( 'NONE', #9438, #9121, #12732 ) ;
#13782 = CARTESIAN_POINT ( 'NONE',  ( 19.99999999999999645, 63.17103598352126426, 16.33561182745161844 ) ) ;
#13783 = EDGE_LOOP ( 'NONE', ( #4440, #4752, #19019, #13349, #5019 ) ) ;
#13784 = CARTESIAN_POINT ( 'NONE',  ( 2.000000000000010658, -3.464101615137748169, 0.000000000000000000 ) ) ;
#13785 = CIRCLE ( 'NONE', #10750, 72.00000000007199219 ) ;
#13786 = CARTESIAN_POINT ( 'NONE',  ( -10.19618095414378622, -15.25966316918061416, -11.15160624981968951 ) ) ;
#13787 = LINE ( 'NONE', #851, #17171 ) ;
#13788 = VERTEX_POINT ( 'NONE', #4787 ) ;
#13789 = FACE_OUTER_BOUND ( 'NONE', #18260, .T. ) ;
#13790 = CIRCLE ( 'NONE', #20201, 23.00000000000000000 ) ;
#13791 = ORIENTED_EDGE ( 'NONE', *, *, #33, .F. ) ;
#13792 = CARTESIAN_POINT ( 'NONE',  ( 9.999999999999998224, -20.34307325858738835, -69.06634035770328239 ) ) ;
#13793 = CARTESIAN_POINT ( 'NONE',  ( 0.000000000000000000, 0.000000000000000000, 5.000000000000000000 ) ) ;
#13794 = CIRCLE ( 'NONE', #3303, 72.00000000007199219 ) ;
#13795 = VERTEX_POINT ( 'NONE', #14643 ) ;
#13796 = EDGE_LOOP ( 'NONE', ( #12146, #19956 ) ) ;
#13797 = CARTESIAN_POINT ( 'NONE',  ( 6.249999999999902300, -10.82531754730554496, -43.00000000000000000 ) ) ;
#13798 = EDGE_CURVE ( 'NONE', #5677, #9154, #5198, .T. ) ;
#13799 = AXIS2_PLACEMENT_3D ( 'NONE', #15131, #11945, #18418 ) ;
#13800 =( NAMED_UNIT ( * ) SI_UNIT ( $, .STERADIAN. ) SOLID_ANGLE_UNIT ( ) );
#13801 = LINE ( 'NONE', #5508, #18729 ) ;
#13802 = AXIS2_PLACEMENT_3D ( 'NONE', #3230, #12988, #8202 ) ;
#13803 = CARTESIAN_POINT ( 'NONE',  ( 85.00002539999999840, 0.000000000000000000, 0.000000000000000000 ) ) ;
#13804 = CIRCLE ( 'NONE', #16506, 65.24900000006525147 ) ;
#13805 = CARTESIAN_POINT ( 'NONE',  ( -9.015947181032828388E-10, -7.500000000000000888, 2.730050000180312075 ) ) ;
#13806 = CARTESIAN_POINT ( 'NONE',  ( 17.50000000000000355, -2.143131898507868643E-15, -43.00000000000000000 ) ) ;
#13807 = CARTESIAN_POINT ( 'NONE',  ( 0.000000000000000000, 27.80658314415226329, 66.41380830714133765 ) ) ;
#13808 = CARTESIAN_POINT ( 'NONE',  ( 30.00000000000001066, 39.99999999999998579, -120.0000000000000142 ) ) ;
#13809 = CARTESIAN_POINT ( 'NONE',  ( 6.250000000000054179, 10.82531754730546147, -40.00000000000000000 ) ) ;
#13810 = EDGE_LOOP ( 'NONE', ( #1028, #20505, #16278, #13095 ) ) ;
#13811 = EDGE_CURVE ( 'NONE', #9645, #12005, #17443, .T. ) ;
#13812 = DIRECTION ( 'NONE',  ( -1.000000000000000000, 0.000000000000000000, 0.000000000000000000 ) ) ;
#13813 = ORIENTED_EDGE ( 'NONE', *, *, #10392, .T. ) ;
#13814 = CARTESIAN_POINT ( 'NONE',  ( -18.00000000043041126, -3.580422610670022543, 6.971918750180314817 ) ) ;
#13815 = CARTESIAN_POINT ( 'NONE',  ( 13.23800900960919158, -16.95692081615699820, 72.71034110640577808 ) ) ;
#13816 = ORIENTED_EDGE ( 'NONE', *, *, #10670, .T. ) ;
#13817 = FACE_OUTER_BOUND ( 'NONE', #12346, .T. ) ;
#13818 = ORIENTED_EDGE ( 'NONE', *, *, #9840, .T. ) ;
#13819 = DIRECTION ( 'NONE',  ( 1.000000000000000000, 0.000000000000000000, 0.000000000000000000 ) ) ;
#13820 = CARTESIAN_POINT ( 'NONE',  ( 0.000000000000000000, -20.34307325858834048, 69.06634035770301239 ) ) ;
#13821 = CARTESIAN_POINT ( 'NONE',  ( 0.000000000000000000, -71.76067541710847308, -5.865617076725382795 ) ) ;
#13822 = VECTOR ( 'NONE', #4049, 1000.000000000000000 ) ;
#13823 = ORIENTED_EDGE ( 'NONE', *, *, #17892, .F. ) ;
#13824 = CARTESIAN_POINT ( 'NONE',  ( -6.358192988180021210, -4.248408729364580694, -17.80739374981969192 ) ) ;
#13825 = DIRECTION ( 'NONE',  ( 0.000000000000000000, 0.000000000000000000, -1.000000000000000000 ) ) ;
#13826 = CARTESIAN_POINT ( 'NONE',  ( 18.00000000043040771, 3.580422610670018546, -16.59058124981969229 ) ) ;
#13827 = FACE_OUTER_BOUND ( 'NONE', #11658, .T. ) ;
#13828 = DIRECTION ( 'NONE',  ( -1.000000000000000000, 0.000000000000000000, 0.000000000000000000 ) ) ;
#13829 = CARTESIAN_POINT ( 'NONE',  ( -11.17563879758428769, -2.222972768810840272, -7.364421499352572731 ) ) ;
#13830 = ORIENTED_EDGE ( 'NONE', *, *, #19688, .F. ) ;
#13831 = CYLINDRICAL_SURFACE ( 'NONE', #2386, 72.00000000007199219 ) ;
#13832 = ORIENTED_EDGE ( 'NONE', *, *, #4791, .T. ) ;
#13833 = CARTESIAN_POINT ( 'NONE',  ( 19.79075590726361966, -8.422956900484598108, -78.26370100276550090 ) ) ;
#13834 = VERTEX_POINT ( 'NONE', #18136 ) ;
#13835 = EDGE_CURVE ( 'NONE', #18949, #19322, #3606, .T. ) ;
#13836 = CARTESIAN_POINT ( 'NONE',  ( 6.888301780572507305, -16.62983158603121936, -12.62426249981968596 ) ) ;
#13837 = DIRECTION ( 'NONE',  ( 1.000000000000000000, 0.000000000000000000, 0.000000000000000000 ) ) ;
#13838 = CARTESIAN_POINT ( 'NONE',  ( 50.00000000000000000, -42.57363661491096707, -121.3828884801879155 ) ) ;
#13839 = ORIENTED_EDGE ( 'NONE', *, *, #11009, .F. ) ;
#13840 = CARTESIAN_POINT ( 'NONE',  ( 30.00000000000000711, -40.00000000000001421, -120.0000000000000142 ) ) ;
#13841 = ORIENTED_EDGE ( 'NONE', *, *, #9043, .T. ) ;
#13842 = CARTESIAN_POINT ( 'NONE',  ( 7.500000000000007105, -2.290195989506637665E-15, 16.06370000000231357 ) ) ;
#13843 = ORIENTED_EDGE ( 'NONE', *, *, #18889, .T. ) ;
#13844 = CARTESIAN_POINT ( 'NONE',  ( 30.84782268423197849, -110.7785652318826237, 73.91276197030045125 ) ) ;
#13845 = DIRECTION ( 'NONE',  ( 0.000000000000000000, 0.000000000000000000, -1.000000000000000000 ) ) ;
#13846 = CONTEXT_DEPENDENT_SHAPE_REPRESENTATION ( #4925, #4266 ) ;
#13847 = CARTESIAN_POINT ( 'NONE',  ( -10.46442989454075878, -10.46442989202484242, 0.4246669188415451712 ) ) ;
#13848 = VERTEX_POINT ( 'NONE', #19412 ) ;
#13849 = CARTESIAN_POINT ( 'NONE',  ( -4.000000000000000000, -0.3902508023145548899, -5.600000000000000533 ) ) ;
#13850 = VERTEX_POINT ( 'NONE', #10083 ) ;
#13851 = CARTESIAN_POINT ( 'NONE',  ( 19.99999999999999645, 63.17103598352126426, 16.33561182745161844 ) ) ;
#13852 = CARTESIAN_POINT ( 'NONE',  ( -17.99999999956958163, 3.580422614997673669, 7.560981250180310198 ) ) ;
#13853 = CARTESIAN_POINT ( 'NONE',  ( 50.00000000000000000, -151.4095880458873467, 44.60680010464249534 ) ) ;
#13854 = CARTESIAN_POINT ( 'NONE',  ( 0.000000000000000000, 0.000000000000000000, 0.000000000000000000 ) ) ;
#13855 = ORIENTED_EDGE ( 'NONE', *, *, #12625, .T. ) ;
#13856 = DIRECTION ( 'NONE',  ( -1.000000000000000000, 0.000000000000000000, 0.000000000000000000 ) ) ;
#13857 = DIRECTION ( 'NONE',  ( 0.000000000000000000, 0.000000000000000000, 1.000000000000000000 ) ) ;
#13858 = ORIENTED_EDGE ( 'NONE', *, *, #18557, .F. ) ;
#13859 = EDGE_CURVE ( 'NONE', #9479, #17758, #16464, .T. ) ;
#13860 = CARTESIAN_POINT ( 'NONE',  ( 22.70866746290765903, -3.649167310370807105, -90.00000000000000000 ) ) ;
#13861 = ORIENTED_EDGE ( 'NONE', *, *, #5836, .F. ) ;
#13862 = CARTESIAN_POINT ( 'NONE',  ( 0.000000000000000000, 0.000000000000000000, 0.000000000000000000 ) ) ;
#13863 = CARTESIAN_POINT ( 'NONE',  ( 10.19618095414378622, 15.25966316918061239, -8.343706249819691223 ) ) ;
#13864 = EDGE_CURVE ( 'NONE', #2489, #8874, #9318, .T. ) ;
#13865 = ORIENTED_EDGE ( 'NONE', *, *, #5772, .F. ) ;
#13866 = VERTEX_POINT ( 'NONE', #6472 ) ;
#13867 = CARTESIAN_POINT ( 'NONE',  ( 30.00000000000000000, -105.0000000000000000, -90.00000000000001421 ) ) ;
#13868 = FACE_OUTER_BOUND ( 'NONE', #5956, .T. ) ;
#13869 = FACE_OUTER_BOUND ( 'NONE', #12140, .T. ) ;
#13870 = DIRECTION ( 'NONE',  ( 1.000000000000000000, 0.000000000000000000, 0.000000000000000000 ) ) ;
#13871 = EDGE_CURVE ( 'NONE', #7712, #19326, #1268, .T. ) ;
#13872 = CARTESIAN_POINT ( 'NONE',  ( -10.19618095414378800, -15.25966316918061771, 7.698393750180310136 ) ) ;
#13873 = ADVANCED_FACE ( 'NONE', ( #11364 ), #9968, .F. ) ;
#13874 = AXIS2_PLACEMENT_3D ( 'NONE', #16820, #704, #16918 ) ;
#13875 = UNCERTAINTY_MEASURE_WITH_UNIT (LENGTH_MEASURE( 1.000000000000000082E-05 ), #2142, 'distance_accuracy_value', 'NONE');
#13876 = CARTESIAN_POINT ( 'NONE',  ( 2.870125741905214412, -6.929096494179682431, -1.019112499819684770 ) ) ;
#13877 =( REPRESENTATION_RELATIONSHIP ('NONE','NONE', #13739, #12383 ) REPRESENTATION_RELATIONSHIP_WITH_TRANSFORMATION ( #11186 )SHAPE_REPRESENTATION_RELATIONSHIP( ) );
#13878 = ORIENTED_EDGE ( 'NONE', *, *, #20155, .F. ) ;
#13879 = CARTESIAN_POINT ( 'NONE',  ( 2.870125741905214412, -6.929096494179682431, 17.83088750018031732 ) ) ;
#13880 = CARTESIAN_POINT ( 'NONE',  ( 1.779017513685135741E-09, 14.79893867758296544, 7.765958081519076295 ) ) ;
#13881 = CARTESIAN_POINT ( 'NONE',  ( 52.50000000000000000, -30.00000000000000000, 5.000000000000000000 ) ) ;
#13882 = EDGE_CURVE ( 'NONE', #1850, #16461, #8551, .T. ) ;
#13883 = ORIENTED_EDGE ( 'NONE', *, *, #20237, .T. ) ;
#13884 = CARTESIAN_POINT ( 'NONE',  ( 7.575000000000064126, 13.12028486733421850, -43.00000000000000000 ) ) ;
#13885 = CARTESIAN_POINT ( 'NONE',  ( 16.62983158437509346, -6.888301784570739272, -13.80238749981968915 ) ) ;
#13886 = CARTESIAN_POINT ( 'NONE',  ( -15.15000000000000568, -3.245314017740485469E-16, -43.00000000000000000 ) ) ;
#13887 = EDGE_LOOP ( 'NONE', ( #15639, #15225, #5898, #19994 ) ) ;
#13888 = EDGE_CURVE ( 'NONE', #7434, #232, #2263, .T. ) ;
#13889 = ORIENTED_EDGE ( 'NONE', *, *, #9467, .T. ) ;
#13890 = CARTESIAN_POINT ( 'NONE',  ( 30.62964503024144491, -40.90928292143731682, -71.38288848018790134 ) ) ;
#13891 = DIRECTION ( 'NONE',  ( -1.000000000000000000, 0.000000000000000000, 0.000000000000000000 ) ) ;
#13892 = ADVANCED_FACE ( 'NONE', ( #13373 ), #4967, .T. ) ;
#13893 = AXIS2_PLACEMENT_3D ( 'NONE', #8797, #18783, #17295 ) ;
#13894 = VERTEX_POINT ( 'NONE', #10291 ) ;
#13895 = VERTEX_POINT ( 'NONE', #16751 ) ;
#13896 = CARTESIAN_POINT ( 'NONE',  ( 24.99999999999999645, -85.00000000000000000, -1.040949779275250179E-14 ) ) ;
#13897 = EDGE_CURVE ( 'NONE', #645, #17111, #7315, .T. ) ;
#13898 = CIRCLE ( 'NONE', #13557, 0.2500000000000002220 ) ;
#13899 = DIRECTION ( 'NONE',  ( 0.000000000000000000, 0.000000000000000000, 1.000000000000000000 ) ) ;
#13900 = CARTESIAN_POINT ( 'NONE',  ( 0.000000000000000000, 0.000000000000000000, 43.00000000000000000 ) ) ;
#13901 = CARTESIAN_POINT ( 'NONE',  ( -6.358192987158591158, 4.248408730893245000, -3.455106249819688724 ) ) ;
#13902 = AXIS2_PLACEMENT_3D ( 'NONE', #14865, #3925, #339 ) ;
#13903 = LINE ( 'NONE', #12104, #5787 ) ;
#13904 = FACE_OUTER_BOUND ( 'NONE', #16128, .T. ) ;
#13905 = EDGE_CURVE ( 'NONE', #4471, #8788, #214, .T. ) ;
#13906 = CARTESIAN_POINT ( 'NONE',  ( 19.99999999999999645, 51.96384592647266487, -49.83732252579562783 ) ) ;
#13907 = DIRECTION ( 'NONE',  ( 0.000000000000000000, 0.6310879443260540844, -0.7757112907044187988 ) ) ;
#13908 = EDGE_CURVE ( 'NONE', #16884, #8077, #19179, .T. ) ;
#13909 = ORIENTED_EDGE ( 'NONE', *, *, #18566, .F. ) ;
#13910 = DIRECTION ( 'NONE',  ( -1.000000000000000000, -0.000000000000000000, -0.000000000000000000 ) ) ;
#13911 = ORIENTED_EDGE ( 'NONE', *, *, #17082, .F. ) ;
#13912 = CARTESIAN_POINT ( 'NONE',  ( 10.19618095047497874, -15.25966317163203279, 4.026606250180313040 ) ) ;
#13913 = CARTESIAN_POINT ( 'NONE',  ( 16.80529800326409173, -13.48305675317432595, 74.69048503828152263 ) ) ;
#13914 = ORIENTED_EDGE ( 'NONE', *, *, #19809, .F. ) ;
#13915 = DIRECTION ( 'NONE',  ( 0.000000000000000000, 0.000000000000000000, 1.000000000000000000 ) ) ;
#13916 = ORIENTED_EDGE ( 'NONE', *, *, #9163, .F. ) ;
#13917 = PRODUCT ( 'hex nut gradec_iso_ISO - 4034 - M5 - N', 'hex nut gradec_iso_ISO - 4034 - M5 - N', '', ( #11511 ) ) ;
#13918 = DIRECTION ( 'NONE',  ( -1.000000000000000000, -0.000000000000000000, -0.000000000000000000 ) ) ;
#13919 = DIRECTION ( 'NONE',  ( 0.000000000000000000, 0.000000000000000000, 1.000000000000000000 ) ) ;
#13920 = DIRECTION ( 'NONE',  ( 0.000000000000000000, 0.000000000000000000, 1.000000000000000000 ) ) ;
#13921 = ADVANCED_FACE ( 'NONE', ( #2436 ), #13479, .T. ) ;
#13922 = ORIENTED_EDGE ( 'NONE', *, *, #6727, .F. ) ;
#13923 = CARTESIAN_POINT ( 'NONE',  ( 40.00000000000000711, -122.3205080756887639, 80.28096411455982206 ) ) ;
#13924 = DIRECTION ( 'NONE',  ( 0.000000000000000000, 0.000000000000000000, -1.000000000000000000 ) ) ;
#13925 = CARTESIAN_POINT ( 'NONE',  ( 2.500000000000000000, -1.178949249685213863, 2.042000000000002924 ) ) ;
#13926 = DIRECTION ( 'NONE',  ( 1.000000000000000000, 0.000000000000000000, 0.000000000000000000 ) ) ;
#13927 = DIRECTION ( 'NONE',  ( 1.000000000000000000, 0.000000000000000000, 0.000000000000000000 ) ) ;
#13928 = AXIS2_PLACEMENT_3D ( 'NONE', #18560, #6889, #13372 ) ;
#13929 = VERTEX_POINT ( 'NONE', #15062 ) ;
#13930 = SURFACE_STYLE_USAGE ( .BOTH. , #9155 ) ;
#13931 = CARTESIAN_POINT ( 'NONE',  ( 0.000000000000000000, 63.85430960833475211, 11.25592921604948948 ) ) ;
#13932 = ORIENTED_EDGE ( 'NONE', *, *, #14431, .T. ) ;
#13933 = VECTOR ( 'NONE', #12198, 1000.000000000000000 ) ;
#13934 = CARTESIAN_POINT ( 'NONE',  ( 12.05832282520466947, -17.81513111787450043, -72.26823280878556943 ) ) ;
#13935 = DIRECTION ( 'NONE',  ( 0.000000000000000000, -1.000000000000000000, 0.000000000000000000 ) ) ;
#13936 = ORIENTED_EDGE ( 'NONE', *, *, #12570, .F. ) ;
#13937 = CARTESIAN_POINT ( 'NONE',  ( -18.00000000000000000, 2.163826221265758884E-09, -19.10394999981969022 ) ) ;
#13938 = DIRECTION ( 'NONE',  ( 0.000000000000000000, 0.000000000000000000, -1.000000000000000000 ) ) ;
#13939 = LINE ( 'NONE', #18710, #15796 ) ;
#13940 = AXIS2_PLACEMENT_3D ( 'NONE', #4359, #10824, #2766 ) ;
#13941 = EDGE_LOOP ( 'NONE', ( #11777, #6940, #8311, #7591 ) ) ;
#13942 = CONICAL_SURFACE ( 'NONE', #9543, 4.000000000000000000, 1.047197551196595855 ) ;
#13943 = CARTESIAN_POINT ( 'NONE',  ( 19.99999999999999645, 27.62776854598856602, 58.65812137499012380 ) ) ;
#13944 = ORIENTED_EDGE ( 'NONE', *, *, #12855, .F. ) ;
#13945 = CARTESIAN_POINT ( 'NONE',  ( -25.00000000000000000, -30.00000000000000711, 58.09475019311124555 ) ) ;
#13946 = VECTOR ( 'NONE', #831, 1000.000000000000000 ) ;
#13947 = VERTEX_POINT ( 'NONE', #2129 ) ;
#13948 = AXIS2_PLACEMENT_3D ( 'NONE', #8409, #4641, #14881 ) ;
#13949 = DIRECTION ( 'NONE',  ( -1.000000000000000000, -0.000000000000000000, 0.000000000000000000 ) ) ;
#13950 = EDGE_CURVE ( 'NONE', #5238, #5869, #10609, .T. ) ;
#13951 = LINE ( 'NONE', #2614, #16008 ) ;
#13952 = ITEM_DEFINED_TRANSFORMATION ( 'NONE', 'NONE', #7270,  #12461 ) ;
#13953 = CARTESIAN_POINT ( 'NONE',  ( 14.79893867758297610, -1.779016607511492805E-09, -3.109708081158454096 ) ) ;
#13954 = AXIS2_PLACEMENT_3D ( 'NONE', #4296, #5887, #1018 ) ;
#13956 = ORIENTED_EDGE ( 'NONE', *, *, #410, .F. ) ;
#13955 = AXIS2_PLACEMENT_3D ( 'NONE', #11480, #6593, #8099 ) ;
#13957 = DIRECTION ( 'NONE',  ( 0.000000000000000000, -0.7308359642781160348, -0.6825531432186625613 ) ) ;
#13958 = CIRCLE ( 'NONE', #5818, 4.000000000000000888 ) ;
#13959 = VERTEX_POINT ( 'NONE', #9015 ) ;
#13960 = CARTESIAN_POINT ( 'NONE',  ( -19.83201477098864274, -8.377285018628274571, 84.88081099966895238 ) ) ;
#13961 = CARTESIAN_POINT ( 'NONE',  ( -6.888301780572500199, 16.62983158603121936, 9.033637500180310198 ) ) ;
#13962 = CARTESIAN_POINT ( 'NONE',  ( 19.99999999999999645, 68.15657073222466522, -23.20952102120210370 ) ) ;
#13963 = CARTESIAN_POINT ( 'NONE',  ( 19.99999999999999645, -3.141410481201533322, 65.17333458706184501 ) ) ;
#13964 = EDGE_LOOP ( 'NONE', ( #18384, #16335, #15620, #16771 ) ) ;
#13965 = CARTESIAN_POINT ( 'NONE',  ( 0.000000000000000000, 0.000000000000000000, 46.00000000000000711 ) ) ;
#13966 = DIRECTION ( 'NONE',  ( 1.000000000000000000, 0.000000000000000000, 0.000000000000000000 ) ) ;
#13967 = ORIENTED_EDGE ( 'NONE', *, *, #1996, .T. ) ;
#13968 = AXIS2_PLACEMENT_3D ( 'NONE', #629, #2210, #18318 ) ;
#13969 = CARTESIAN_POINT ( 'NONE',  ( 18.48989557468869549, -13.69507619692709710, -80.56043633723008668 ) ) ;
#13970 = VECTOR ( 'NONE', #18971, 1000.000000000000000 ) ;
#13971 = CARTESIAN_POINT ( 'NONE',  ( 24.74873734152916072, 24.74873734152916072, -120.0000000000000142 ) ) ;
#13972 = CARTESIAN_POINT ( 'NONE',  ( 3.580422610670019878, -18.00000000043040771, -4.809331249819689624 ) ) ;
#13973 = EDGE_LOOP ( 'NONE', ( #12454, #14568 ) ) ;
#13974 = CIRCLE ( 'NONE', #9905, 4.250000000000000000 ) ;
#13975 = ORIENTED_EDGE ( 'NONE', *, *, #2819, .F. ) ;
#13976 = FACE_OUTER_BOUND ( 'NONE', #7742, .T. ) ;
#13977 = DIRECTION ( 'NONE',  ( 1.000000000000000000, 0.000000000000000000, 0.000000000000000000 ) ) ;
#13978 = ADVANCED_FACE ( 'NONE', ( #11869, #18339 ), #2554, .F. ) ;
#13979 = CYLINDRICAL_SURFACE ( 'NONE', #8515, 65.24900000006525147 ) ;
#13980 = DIRECTION ( 'NONE',  ( -1.000000000000000000, -0.000000000000000000, 0.000000000000000000 ) ) ;
#13981 = DIRECTION ( 'NONE',  ( 0.000000000000000000, 0.000000000000000000, 1.000000000000000000 ) ) ;
#13982 = AXIS2_PLACEMENT_3D ( 'NONE', #20520, #8969, #2712 ) ;
#13983 = CARTESIAN_POINT ( 'NONE',  ( 18.00000000043041481, 3.580422610670020322, 13.58901875018030836 ) ) ;
#13984 = CARTESIAN_POINT ( 'NONE',  ( 5.303300858261588147, -5.303300859536636658, -11.03317499981968552 ) ) ;
#13985 = ORIENTED_EDGE ( 'NONE', *, *, #18633, .F. ) ;
#13986 = CIRCLE ( 'NONE', #1784, 72.00000000007199219 ) ;
#13987 = DIRECTION ( 'NONE',  ( -1.000000000000000000, 0.000000000000000000, 0.000000000000000000 ) ) ;
#13988 = EDGE_CURVE ( 'NONE', #1468, #14604, #15483, .T. ) ;
#13989 = VECTOR ( 'NONE', #12924, 1000.000000000000000 ) ;
#13990 = CARTESIAN_POINT ( 'NONE',  ( 14.79893867793683349, 2.943691925285396582, 9.827676831519074341 ) ) ;
#13991 = CARTESIAN_POINT ( 'NONE',  ( 6.680000000000001492, -11.17999999999998550, 1.369155121446739974E-15 ) ) ;
#13992 = ORIENTED_EDGE ( 'NONE', *, *, #1103, .T. ) ;
#13993 = CARTESIAN_POINT ( 'NONE',  ( 19.99999999999999645, 0.000000000000000000, 0.000000000000000000 ) ) ;
#13994 = DIRECTION ( 'NONE',  ( 0.000000000000000000, 0.000000000000000000, 1.000000000000000000 ) ) ;
#13995 = CYLINDRICAL_SURFACE ( 'NONE', #13447, 11.49999999999999645 ) ;
#13996 = AXIS2_PLACEMENT_3D ( 'NONE', #14727, #11230, #19279 ) ;
#13997 = EDGE_LOOP ( 'NONE', ( #19627, #5642, #9073, #4405 ) ) ;
#13998 = EDGE_CURVE ( 'NONE', #1069, #17642, #12768, .T. ) ;
#13999 = VECTOR ( 'NONE', #7314, 1000.000000000000000 ) ;
#14000 = DIRECTION ( 'NONE',  ( -1.000000000000000000, -0.000000000000000000, 0.000000000000000000 ) ) ;
#14001 = VERTEX_POINT ( 'NONE', #20130 ) ;
#14002 = DIRECTION ( 'NONE',  ( -1.000000000000000000, 0.000000000000000000, 0.000000000000000000 ) ) ;
#14003 = CARTESIAN_POINT ( 'NONE',  ( 0.000000000000000000, 2.357898499370431722, -2.818925648462311528E-15 ) ) ;
#14004 = ORIENTED_EDGE ( 'NONE', *, *, #17793, .F. ) ;
#14005 = VERTEX_POINT ( 'NONE', #18561 ) ;
#14006 = CARTESIAN_POINT ( 'NONE',  ( 17.50000000000000355, 2.143131898507868643E-15, 46.00000000000000711 ) ) ;
#14007 = CIRCLE ( 'NONE', #4856, 27.60000000002760245 ) ;
#14008 = VECTOR ( 'NONE', #6802, 1000.000000000000000 ) ;
#14009 = CARTESIAN_POINT ( 'NONE',  ( 0.000000000000000000, 0.000000000000000000, 4.000000000000000000 ) ) ;
#14010 = DIRECTION ( 'NONE',  ( -1.000000000000000000, 0.000000000000000000, 0.000000000000000000 ) ) ;
#14011 = CIRCLE ( 'NONE', #2157, 0.06721999999999977993 ) ;
#14012 = CIRCLE ( 'NONE', #8576, 17.50000000000000355 ) ;
#14013 = ADVANCED_FACE ( 'NONE', ( #4016, #10497, #15375, #6890, #856, #7309 ), #5303, .T. ) ;
#14014 = AXIS2_PLACEMENT_3D ( 'NONE', #18920, #7678, #15839 ) ;
#14015 = CARTESIAN_POINT ( 'NONE',  ( 5.303300859536630441, 5.303300858261584594, -19.65432499981969272 ) ) ;
#14016 = ADVANCED_FACE ( 'NONE', ( #15791 ), #10718, .T. ) ;
#14017 = SURFACE_SIDE_STYLE ('',( #17083 ) ) ;
#14018 = FACE_OUTER_BOUND ( 'NONE', #11220, .T. ) ;
#14019 = CARTESIAN_POINT ( 'NONE',  ( 19.99999999999999645, 0.000000000000000000, 0.000000000000000000 ) ) ;
#14020 = AXIS2_PLACEMENT_3D ( 'NONE', #20261, #2887, #5738 ) ;
#14021 = VECTOR ( 'NONE', #4501, 1000.000000000000000 ) ;
#14022 = ORIENTED_EDGE ( 'NONE', *, *, #8676, .F. ) ;
#14023 = CARTESIAN_POINT ( 'NONE',  ( -10.00000000000000000, 0.000000000000000000, 0.000000000000000000 ) ) ;
#14024 = VERTEX_POINT ( 'NONE', #2757 ) ;
#14025 = EDGE_CURVE ( 'NONE', #11443, #20609, #2602, .T. ) ;
#14026 = CARTESIAN_POINT ( 'NONE',  ( -15.25966316918061771, 10.19618095414378622, -10.69995624981968518 ) ) ;
#14027 = LINE ( 'NONE', #18902, #18781 ) ;
#14028 = EDGE_CURVE ( 'NONE', #19208, #1859, #17391, .T. ) ;
#14029 = VERTEX_POINT ( 'NONE', #17601 ) ;
#14030 = CARTESIAN_POINT ( 'NONE',  ( 3.600000000000066702, 10.82531754730546147, 166.0000000000000000 ) ) ;
#14031 = VERTEX_POINT ( 'NONE', #9223 ) ;
#14032 = PLANE ( 'NONE',  #7808 ) ;
#14033 = CYLINDRICAL_SURFACE ( 'NONE', #9729, 7.500000000000000000 ) ;
#14034 = CARTESIAN_POINT ( 'NONE',  ( 4.248408730893246776, 6.358192987158592047, -1.098856249819691433 ) ) ;
#14035 = AXIS2_PLACEMENT_3D ( 'NONE', #12864, #12661, #6282 ) ;
#14036 = ORIENTED_EDGE ( 'NONE', *, *, #13401, .T. ) ;
#14037 = PLANE ( 'NONE',  #7988 ) ;
#14038 = CARTESIAN_POINT ( 'NONE',  ( 2.500000000000000000, -2.357898499370432610, 3.252606517456513302E-15 ) ) ;
#14039 = FACE_OUTER_BOUND ( 'NONE', #18139, .T. ) ;
#14040 = VECTOR ( 'NONE', #8095, 1000.000000000000000 ) ;
#14041 = DIRECTION ( 'NONE',  ( -1.000000000000000000, 0.000000000000000000, 0.000000000000000000 ) ) ;
#14042 = ADVANCED_FACE ( 'NONE', ( #1295 ), #15685, .T. ) ;
#14043 = VECTOR ( 'NONE', #14, 1000.000000000000000 ) ;
#14044 = CARTESIAN_POINT ( 'NONE',  ( 50.00000000000000000, -97.49621075554985339, -111.6458212409894486 ) ) ;
#14045 = EDGE_LOOP ( 'NONE', ( #1678, #12411, #15730, #10492 ) ) ;
#14046 = CARTESIAN_POINT ( 'NONE',  ( -31.74999999999995737, 0.000000000000000000, 0.000000000000000000 ) ) ;
#14047 = EDGE_CURVE ( 'NONE', #9722, #16972, #1926, .T. ) ;
#14048 = CARTESIAN_POINT ( 'NONE',  ( 19.99999999999999645, 0.000000000000000000, 0.000000000000000000 ) ) ;
#14049 = ORIENTED_EDGE ( 'NONE', *, *, #13351, .F. ) ;
#14050 = CARTESIAN_POINT ( 'NONE',  ( 19.99999999999999645, -24.01204443665145405, -60.22865198596149838 ) ) ;
#14051 = CARTESIAN_POINT ( 'NONE',  ( 7.574999999999881162, -13.12028486733431976, -43.00000000000000000 ) ) ;
#14052 = EDGE_CURVE ( 'NONE', #12808, #9351, #17507, .T. ) ;
#14053 = EDGE_LOOP ( 'NONE', ( #1171, #7520 ) ) ;
#14054 = CARTESIAN_POINT ( 'NONE',  ( -3.580422614997675002, -17.99999999956958163, -21.16566874981968738 ) ) ;
#14055 = DIRECTION ( 'NONE',  ( -1.648349939164583742E-16, 1.000000000000000000, 0.000000000000000000 ) ) ;
#14056 = DIRECTION ( 'NONE',  ( 0.000000000000000000, 0.000000000000000000, 1.000000000000000000 ) ) ;
#14057 = EDGE_LOOP ( 'NONE', ( #11246, #13173, #20424, #2552 ) ) ;
#14058 = CARTESIAN_POINT ( 'NONE',  ( 19.99999999999999645, 0.000000000000000000, 0.000000000000000000 ) ) ;
#14059 = ORIENTED_EDGE ( 'NONE', *, *, #10612, .T. ) ;
#14060 = PLANE ( 'NONE',  #9542 ) ;
#14061 = EDGE_LOOP ( 'NONE', ( #9855, #8106, #14070, #15064, #2995, #18993 ) ) ;
#14062 = CARTESIAN_POINT ( 'NONE',  ( -5.303300858261584594, 5.303300859536631329, 6.264425000180307457 ) ) ;
#14063 = DIRECTION ( 'NONE',  ( 0.000000000000000000, 0.000000000000000000, 1.000000000000000000 ) ) ;
#14064 = ADVANCED_FACE ( 'NONE', ( #4669 ), #18978, .T. ) ;
#14065 = DIRECTION ( 'NONE',  ( 0.000000000000000000, 0.9422609221188191775, 0.3348796121709899376 ) ) ;
#14066 = CARTESIAN_POINT ( 'NONE',  ( -14.79893867758297610, 1.779018419858781159E-09, -7.822208081158454895 ) ) ;
#14067 = EDGE_LOOP ( 'NONE', ( #146, #10792 ) ) ;
#14068 = AXIS2_PLACEMENT_3D ( 'NONE', #11059, #4273, #15924 ) ;
#14069 = CARTESIAN_POINT ( 'NONE',  ( 0.000000000000000000, 0.000000000000000000, 166.0000000000000000 ) ) ;
#14070 = ORIENTED_EDGE ( 'NONE', *, *, #6011, .T. ) ;
#14071 = CARTESIAN_POINT ( 'NONE',  ( 19.99999999999999645, 14.55863677812212131, -63.60407295269091321 ) ) ;
#14072 = CARTESIAN_POINT ( 'NONE',  ( -10.19618095414378445, -15.25966316918061239, 15.21879375018031055 ) ) ;
#14073 = CARTESIAN_POINT ( 'NONE',  ( 4.248408730893246776, 6.358192987158592047, -19.94885624981969841 ) ) ;
#14074 = DIRECTION ( 'NONE',  ( -1.000000000000000000, -0.000000000000000000, -0.000000000000000000 ) ) ;
#14075 = ORIENTED_EDGE ( 'NONE', *, *, #15550, .F. ) ;
#14076 = EDGE_CURVE ( 'NONE', #19592, #540, #14788, .T. ) ;
#14077 = CIRCLE ( 'NONE', #16767, 80.00000000000000000 ) ;
#14078 = CARTESIAN_POINT ( 'NONE',  ( 6.359999999999997655, 7.000462221625649605E-15, 0.000000000000000000 ) ) ;
#14079 = DIRECTION ( 'NONE',  ( 0.000000000000000000, 0.000000000000000000, -1.000000000000000000 ) ) ;
#14080 = ORIENTED_EDGE ( 'NONE', *, *, #11678, .F. ) ;
#14081 = DIRECTION ( 'NONE',  ( 0.000000000000000000, 0.000000000000000000, 1.000000000000000000 ) ) ;
#14082 = AXIS2_PLACEMENT_3D ( 'NONE', #3193, #8, #12948 ) ;
#14083 = CARTESIAN_POINT ( 'NONE',  ( -8.500000000000000000, 1.040949779275250140E-15, 81.99999999999998579 ) ) ;
#14084 = CARTESIAN_POINT ( 'NONE',  ( 16.62983158437509346, -6.888301784570737496, -6.281987499819692289 ) ) ;
#14085 = ORIENTED_EDGE ( 'NONE', *, *, #9206, .F. ) ;
#14086 = DIRECTION ( 'NONE',  ( 0.000000000000000000, 0.000000000000000000, 1.000000000000000000 ) ) ;
#14087 = PLANE ( 'NONE',  #1078 ) ;
#14088 = CARTESIAN_POINT ( 'NONE',  ( -24.99999999999999289, 31.35083268962919689, -84.99999999999998579 ) ) ;
#14089 = LINE ( 'NONE', #3998, #6835 ) ;
#14090 = CARTESIAN_POINT ( 'NONE',  ( -2.032919063319296788E-31, 1.106706143828131442E-15, -74.99999999999998579 ) ) ;
#14091 = CARTESIAN_POINT ( 'NONE',  ( 2.163825119083639947E-09, 18.00000000000000355, 11.52730000018030942 ) ) ;
#14092 = CIRCLE ( 'NONE', #9698, 4.000000000000000888 ) ;
#14093 = CARTESIAN_POINT ( 'NONE',  ( 2.870125741905214412, -6.929096494179682431, -19.86911249981968552 ) ) ;
#14094 = ORIENTED_EDGE ( 'NONE', *, *, #14930, .T. ) ;
#14095 = DIRECTION ( 'NONE',  ( 0.000000000000000000, -1.000000000000000000, 1.287488025362403787E-15 ) ) ;
#14096 = CIRCLE ( 'NONE', #6677, 10.85999999999999410 ) ;
#14097 = AXIS2_PLACEMENT_3D ( 'NONE', #9958, #14541, #3300 ) ;
#14098 = CARTESIAN_POINT ( 'NONE',  ( -13.67243654642775041, 5.663308650141531508, 5.998770581519074163 ) ) ;
#14099 = CARTESIAN_POINT ( 'NONE',  ( 24.99999999999999645, -99.99999999999998579, 52.00000000000000000 ) ) ;
#14100 = ORIENTED_EDGE ( 'NONE', *, *, #6761, .F. ) ;
#14101 = EDGE_CURVE ( 'NONE', #7589, #10176, #2664, .T. ) ;
#14102 = CARTESIAN_POINT ( 'NONE',  ( -31.75000000000000000, -11.49999999999999467, 1.408343819019455584E-15 ) ) ;
#14103 = TOROIDAL_SURFACE ( 'NONE', #19549, 7.567219999999999835, 0.06721999999999977993 ) ;
#14104 = CARTESIAN_POINT ( 'NONE',  ( 18.00000000000000000, -2.163824016901520184E-09, -14.39144999981968986 ) ) ;
#14105 = DIRECTION ( 'NONE',  ( 1.000000000000000000, -0.000000000000000000, -0.000000000000000000 ) ) ;
#14106 = ORIENTED_EDGE ( 'NONE', *, *, #2323, .F. ) ;
#14107 = DIRECTION ( 'NONE',  ( -1.000000000000000000, 0.000000000000000000, 0.000000000000000000 ) ) ;
#14108 = ORIENTED_EDGE ( 'NONE', *, *, #7638, .F. ) ;
#14109 = CARTESIAN_POINT ( 'NONE',  ( 38.55055242192437959, -18.08242209349172924, -77.76562703327597603 ) ) ;
#14110 = DIRECTION ( 'NONE',  ( -0.000000000000000000, -0.000000000000000000, 1.000000000000000000 ) ) ;
#14111 = AXIS2_PLACEMENT_3D ( 'NONE', #7955, #7745, #6358 ) ;
#14112 = ORIENTED_EDGE ( 'NONE', *, *, #2205, .F. ) ;
#14113 = EDGE_LOOP ( 'NONE', ( #351, #12426, #19889, #1988 ) ) ;
#14114 = CARTESIAN_POINT ( 'NONE',  ( 38.52966308413987662, -121.3895969659597398, -79.56471955312994737 ) ) ;
#14115 = CIRCLE ( 'NONE', #1589, 65.24900000006526568 ) ;
#14116 = CIRCLE ( 'NONE', #3266, 4.000000000000000000 ) ;
#14117 = COLOUR_RGB ( '', 0.72549020, 0.75294118, 0.79215686) ;
#14118 = DIRECTION ( 'NONE',  ( 0.000000000000000000, 0.000000000000000000, 1.000000000000000000 ) ) ;
#14119 = VECTOR ( 'NONE', #2581, 1000.000000000000000 ) ;
#14120 = FILL_AREA_STYLE ('',( #7640 ) ) ;
#14121 = CARTESIAN_POINT ( 'NONE',  ( -10.32494394809439164, -4.276731812588563386, 13.49332774971320248 ) ) ;
#14122 = VECTOR ( 'NONE', #1505, 1000.000000000000000 ) ;
#14123 =( BOUNDED_CURVE ( )  B_SPLINE_CURVE ( 2, ( #8215, #13203, #14588, #1565, #11301, #16486, #19559, #3441, #4935, #4729, #20935, #14692, #3240, #17666, #6318, #1669, #5035, #11606, #8116, #61, #17972, #6516, #13000, #19453, #19652, #9909, #1864, #275, #6723, #11912, #684, #8738, #3961, #369, #7244, #488, #15205, #3650, #13310, #6934, #3744, #794, #10441, #2176, #11715, #5246, #13726, #16903, #16686, #17003, #18600, #6823, #18494, #2379, #2490, #7133, #8832, #5347, #13617, #20174, #5548, #19763, #5440, #20066, #8630, #18185, #8519, #11814, #15307, #2063, #5660, #10543, #14893, #18385, #12025, #18277, #15000, #10124, #15104, #13419, #4061, #16794, #12133, #16577, #19872, #10225, #592, #2280, #7040, #13518, #19961, #3854, #10332, #19021, #15417, #1336, #15519, #9272, #18707, #7356, #1012, #7681, #15843, #4498, #17227, #5758, #20279, #7780, #10964, #10766, #11076, #12673, #904, #12556, #17440, #17553, #15734, #2911, #20392, #1233, #14255, #2698, #13836, #20502, #14160, #9164, #12233, #2601, #5878, #9381, #17116, #20700, #4605, #8950, #5981, #20603, #12351, #9067, #4178, #15621, #7456, #10659, #10857, #6187, #13937, #18816, #4287, #1123, #17328, #19133, #7569, #14054, #12456, #18924, #4389, #2804, #6080, #14666, #5107, #11172, #16158 ),
 .UNSPECIFIED., .F., .T. ) 
 B_SPLINE_CURVE_WITH_KNOTS ( ( 3, 2, 2, 2, 2, 2, 2, 2, 2, 2, 2, 2, 2, 2, 2, 2, 2, 2, 2, 2, 2, 2, 2, 2, 2, 2, 2, 2, 2, 2, 2, 2, 2, 2, 2, 2, 2, 2, 2, 2, 2, 2, 2, 2, 2, 2, 2, 2, 2, 2, 2, 2, 2, 2, 2, 2, 2, 2, 2, 2, 2, 2, 2, 2, 2, 2, 2, 2, 2, 2, 2, 2, 2, 2, 2, 2, 2, 2, 2, 2, 3 ),
 ( 0.000000000000000000, 0.01250000000000000069, 0.02500000000000000139, 0.03749999999999999861, 0.05000000000000000278, 0.06250000000000000000, 0.07499999999999999722, 0.08749999999999999445, 0.1000000000000000056, 0.1125000000000000028, 0.1250000000000000000, 0.1375000000000000111, 0.1499999999999999944, 0.1625000000000000056, 0.1749999999999999889, 0.1875000000000000000, 0.2000000000000000111, 0.2124999999999999944, 0.2250000000000000056, 0.2374999999999999889, 0.2500000000000000000, 0.2625000000000000111, 0.2750000000000000222, 0.2874999999999999778, 0.2999999999999999889, 0.3125000000000000000, 0.3250000000000000111, 0.3375000000000000222, 0.3499999999999999778, 0.3624999999999999889, 0.3750000000000000000, 0.3875000000000000111, 0.4000000000000000222, 0.4124999999999999778, 0.4249999999999999889, 0.4375000000000000000, 0.4500000000000000111, 0.4625000000000000222, 0.4749999999999999778, 0.4874999999999999889, 0.5000000000000000000, 0.5124999999999999556, 0.5250000000000000222, 0.5374999999999999778, 0.5500000000000000444, 0.5625000000000000000, 0.5749999999999999556, 0.5875000000000000222, 0.5999999999999999778, 0.6125000000000000444, 0.6250000000000000000, 0.6374999999999999556, 0.6500000000000000222, 0.6624999999999999778, 0.6750000000000000444, 0.6875000000000000000, 0.6999999999999999556, 0.7125000000000000222, 0.7249999999999999778, 0.7375000000000000444, 0.7500000000000000000, 0.7624999999999999556, 0.7750000000000000222, 0.7874999999999999778, 0.8000000000000000444, 0.8125000000000000000, 0.8249999999999999556, 0.8375000000000000222, 0.8499999999999999778, 0.8625000000000000444, 0.8750000000000000000, 0.8874999999999999556, 0.9000000000000000222, 0.9124999999999999778, 0.9250000000000000444, 0.9375000000000000000, 0.9499999999999999556, 0.9625000000000000222, 0.9749999999999999778, 0.9875000000000000444, 1.000000000000000000 ),
 .UNSPECIFIED. ) 
 CURVE ( )  GEOMETRIC_REPRESENTATION_ITEM ( )  RATIONAL_B_SPLINE_CURVE ( ( 1.000000000000000000, 0.9807852804032304306, 1.000000000000000000, 0.9807852804032304306, 1.000000000000000000, 0.9807852804032304306, 1.000000000000000000, 0.9807852804032304306, 1.000000000000000000, 0.9807852804032304306, 1.000000000000000000, 0.9807852804032304306, 1.000000000000000000, 0.9807852804032304306, 1.000000000000000000, 0.9807852804032304306, 1.000000000000000000, 0.9807852804032304306, 1.000000000000000000, 0.9807852804032304306, 1.000000000000000000, 0.9807852804032304306, 1.000000000000000000, 0.9807852804032304306, 1.000000000000000000, 0.9807852804032304306, 1.000000000000000000, 0.9807852804032304306, 1.000000000000000000, 0.9807852804032304306, 1.000000000000000000, 0.9807852804032304306, 1.000000000000000000, 0.9807852804032304306, 1.000000000000000000, 0.9807852804032304306, 1.000000000000000000, 0.9807852804032304306, 1.000000000000000000, 0.9807852804032304306, 1.000000000000000000, 0.9807852804032304306, 1.000000000000000000, 0.9807852804032304306, 1.000000000000000000, 0.9807852804032304306, 1.000000000000000000, 0.9807852804032304306, 1.000000000000000000, 0.9807852804032304306, 1.000000000000000000, 0.9807852804032304306, 1.000000000000000000, 0.9807852804032304306, 1.000000000000000000, 0.9807852804032304306, 1.000000000000000000, 0.9807852804032304306, 1.000000000000000000, 0.9807852804032304306, 1.000000000000000000, 0.9807852804032304306, 1.000000000000000000, 0.9807852804032304306, 1.000000000000000000, 0.9807852804032304306, 1.000000000000000000, 0.9807852804032304306, 1.000000000000000000, 0.9807852804032304306, 1.000000000000000000, 0.9807852804032304306, 1.000000000000000000, 0.9807852804032304306, 1.000000000000000000, 0.9807852804032304306, 1.000000000000000000, 0.9807852804032304306, 1.000000000000000000, 0.9807852804032304306, 1.000000000000000000, 0.9807852804032304306, 1.000000000000000000, 0.9807852804032304306, 1.000000000000000000, 0.9807852804032304306, 1.000000000000000000, 0.9807852804032304306, 1.000000000000000000, 0.9807852804032304306, 1.000000000000000000, 0.9807852804032304306, 1.000000000000000000, 0.9807852804032304306, 1.000000000000000000, 0.9807852804032304306, 1.000000000000000000, 0.9807852804032304306, 1.000000000000000000, 0.9807852804032304306, 1.000000000000000000, 0.9807852804032304306, 1.000000000000000000, 0.9807852804032304306, 1.000000000000000000, 0.9807852804032304306, 1.000000000000000000, 0.9807852804032304306, 1.000000000000000000, 0.9807852804032304306, 1.000000000000000000, 0.9807852804032304306, 1.000000000000000000, 0.9807852804032304306, 1.000000000000000000, 0.9807852804032304306, 1.000000000000000000, 0.9807852804032304306, 1.000000000000000000, 0.9807852804032304306, 1.000000000000000000, 0.9807852804032304306, 1.000000000000000000, 0.9807852804032304306, 1.000000000000000000, 0.9807852804032304306, 1.000000000000000000, 0.9807852804032304306, 1.000000000000000000, 0.9807852804032304306, 1.000000000000000000, 0.9807852804032304306, 1.000000000000000000, 0.9807852804032304306, 1.000000000000000000, 0.9807852804032304306, 1.000000000000000000, 0.9807852804032304306, 1.000000000000000000, 0.9807852804032304306, 1.000000000000000000, 0.9807852804032304306, 1.000000000000000000, 0.9807852804032304306, 1.000000000000000000, 0.9807852804032304306, 1.000000000000000000, 0.9807852804032304306, 1.000000000000000000, 0.9807852804032304306, 1.000000000000000000, 0.9807852804032304306, 1.000000000000000000, 0.9807852804032304306, 1.000000000000000000, 0.9807852804032304306, 1.000000000000000000, 0.9807852804032304306, 1.000000000000000000, 0.9807852804032304306, 1.000000000000000000 ) ) 
 REPRESENTATION_ITEM ( '' )  );
#14124 = CARTESIAN_POINT ( 'NONE',  ( -24.99999999999999289, -127.3290820621008379, 85.00000000000000000 ) ) ;
#14125 = CARTESIAN_POINT ( 'NONE',  ( 19.99999999999999645, 64.44931368725534071, -10.18420179740539666 ) ) ;
#14126 = CIRCLE ( 'NONE', #14799, 72.00000000007199219 ) ;
#14127 = ORIENTED_EDGE ( 'NONE', *, *, #5026, .F. ) ;
#14128 = CARTESIAN_POINT ( 'NONE',  ( 19.99999999999999645, 0.000000000000000000, 0.000000000000000000 ) ) ;
#14129 = ORIENTED_EDGE ( 'NONE', *, *, #5189, .F. ) ;
#14130 = CARTESIAN_POINT ( 'NONE',  ( 12.72792205982779734, -12.72792206288791128, -24.54292499981968945 ) ) ;
#14131 = DIRECTION ( 'NONE',  ( -1.000000000000000000, 1.734723475976807094E-16, 0.000000000000000000 ) ) ;
#14132 = ORIENTED_EDGE ( 'NONE', *, *, #2912, .T. ) ;
#14133 = DIRECTION ( 'NONE',  ( -1.000000000000000000, 0.000000000000000000, 0.000000000000000000 ) ) ;
#14134 = ORIENTED_EDGE ( 'NONE', *, *, #49, .F. ) ;
#14135 = CARTESIAN_POINT ( 'NONE',  ( 30.00000000000000000, -151.4095880458873467, 44.60680010464249534 ) ) ;
#14136 = DIRECTION ( 'NONE',  ( -1.000000000000000000, -0.000000000000000000, -0.000000000000000000 ) ) ;
#14137 = CARTESIAN_POINT ( 'NONE',  ( 19.99999999999999645, 64.36139404986009538, -32.27399814043807424 ) ) ;
#14138 = AXIS2_PLACEMENT_3D ( 'NONE', #16827, #16514, #8760 ) ;
#14139 = ORIENTED_EDGE ( 'NONE', *, *, #12244, .T. ) ;
#14140 = EDGE_CURVE ( 'NONE', #1332, #13598, #10604, .T. ) ;
#14141 = CARTESIAN_POINT ( 'NONE',  ( 8.899999999999895550, -10.82531754730554496, 169.0000000000000000 ) ) ;
#14142 = EDGE_CURVE ( 'NONE', #15600, #3649, #10262, .T. ) ;
#14143 = CIRCLE ( 'NONE', #11085, 3.199999999999994404 ) ;
#14144 = EDGE_CURVE ( 'NONE', #16612, #7823, #2822, .T. ) ;
#14145 = DIRECTION ( 'NONE',  ( -1.000000000000000000, -0.000000000000000000, -0.000000000000000000 ) ) ;
#14146 = DIRECTION ( 'NONE',  ( -1.000000000000000000, 0.000000000000000000, 0.000000000000000000 ) ) ;
#14147 = CARTESIAN_POINT ( 'NONE',  ( -24.99999999999999289, -148.4917293642369884, -48.67032260359990659 ) ) ;
#14148 = VECTOR ( 'NONE', #17796, 1000.000000000000000 ) ;
#14149 = CARTESIAN_POINT ( 'NONE',  ( 7.500000000000000888, -1.491842755816072952, 10.09333125008778964 ) ) ;
#14150 = EDGE_CURVE ( 'NONE', #13416, #9221, #7517, .T. ) ;
#14151 = ORIENTED_EDGE ( 'NONE', *, *, #4817, .T. ) ;
#14152 = DIRECTION ( 'NONE',  ( -1.000000000000000000, 0.000000000000000000, 0.000000000000000000 ) ) ;
#14153 = CARTESIAN_POINT ( 'NONE',  ( 19.99999999999999645, -11.98658579560543025, -64.13855129306480762 ) ) ;
#14154 = ORIENTED_EDGE ( 'NONE', *, *, #9340, .F. ) ;
#14155 = AXIS2_PLACEMENT_3D ( 'NONE', #10640, #13502, #12007 ) ;
#14156 = DIRECTION ( 'NONE',  ( 1.000000000000000000, -0.000000000000000000, -0.000000000000000000 ) ) ;
#14157 = FACE_BOUND ( 'NONE', #1814, .T. ) ;
#14158 = VERTEX_POINT ( 'NONE', #9328 ) ;
#14159 = VECTOR ( 'NONE', #5996, 999.9999999999997726 ) ;
#14160 = CARTESIAN_POINT ( 'NONE',  ( 12.72792205982779734, -12.72792206288791128, -13.21332499981968667 ) ) ;
#14161 = FACE_OUTER_BOUND ( 'NONE', #19306, .T. ) ;
#14162 = CARTESIAN_POINT ( 'NONE',  ( 5.000000000000004441, 0.000000000000000000, 0.000000000000000000 ) ) ;
#14163 = ORIENTED_EDGE ( 'NONE', *, *, #13772, .F. ) ;
#14164 = EDGE_CURVE ( 'NONE', #13959, #16282, #18388, .T. ) ;
#14165 = VECTOR ( 'NONE', #17900, 1000.000000000000000 ) ;
#14166 = CARTESIAN_POINT ( 'NONE',  ( 19.99999999999999645, -35.35772184876843482, -54.34979580218228534 ) ) ;
#14167 = ORIENTED_EDGE ( 'NONE', *, *, #14681, .F. ) ;
#14168 = CARTESIAN_POINT ( 'NONE',  ( 0.000000000000000000, 0.000000000000000000, 0.000000000000000000 ) ) ;
#14169 = ORIENTED_EDGE ( 'NONE', *, *, #3910, .T. ) ;
#14170 = EDGE_CURVE ( 'NONE', #13763, #5352, #14675, .T. ) ;
#14171 = EDGE_CURVE ( 'NONE', #20704, #2621, #11021, .T. ) ;
#14172 = CARTESIAN_POINT ( 'NONE',  ( 34.75286706568503803, -117.9715115446175275, 77.27478996839415970 ) ) ;
#14173 = EDGE_CURVE ( 'NONE', #5249, #14524, #11284, .T. ) ;
#14174 = FACE_OUTER_BOUND ( 'NONE', #6351, .T. ) ;
#14175 = ITEM_DEFINED_TRANSFORMATION ( 'NONE', 'NONE', #13389,  #12461 ) ;
#14176 = CARTESIAN_POINT ( 'NONE',  ( -2.943691928843437999, -14.79893867722910450, -9.883926831158460047 ) ) ;
#14177 = VERTEX_POINT ( 'NONE', #1390 ) ;
#14178 = FACE_OUTER_BOUND ( 'NONE', #15518, .T. ) ;
#14179 = FACE_OUTER_BOUND ( 'NONE', #6297, .T. ) ;
#14180 = EDGE_LOOP ( 'NONE', ( #327, #848 ) ) ;
#14181 = CARTESIAN_POINT ( 'NONE',  ( -4.248408730893246776, -6.358192987158592047, -24.66135624981969698 ) ) ;
#14182 = CARTESIAN_POINT ( 'NONE',  ( -18.00000000043040771, -3.580422610670021211, 6.971918750180310376 ) ) ;
#14183 = DIRECTION ( 'NONE',  ( 0.000000000000000000, 0.000000000000000000, -1.000000000000000000 ) ) ;
#14184 = DIRECTION ( 'NONE',  ( 0.000000000000000000, 0.000000000000000000, -1.000000000000000000 ) ) ;
#14185 = ADVANCED_FACE ( 'NONE', ( #7838 ), #14320, .T. ) ;
#14186 = ORIENTED_EDGE ( 'NONE', *, *, #19197, .T. ) ;
#14187 = DIRECTION ( 'NONE',  ( 0.000000000000000000, 0.000000000000000000, -1.000000000000000000 ) ) ;
#14188 = CYLINDRICAL_SURFACE ( 'NONE', #3313, 11.50000000000000000 ) ;
#14189 = VERTEX_POINT ( 'NONE', #4975 ) ;
#14190 = CYLINDRICAL_SURFACE ( 'NONE', #2117, 2.500000000000002220 ) ;
#14191 = DIRECTION ( 'NONE',  ( 0.000000000000000000, 0.9422609221188191775, 0.3348796121709901041 ) ) ;
#14192 = CARTESIAN_POINT ( 'NONE',  ( -17.99999999999999645, 2.163826221265758470E-09, -11.58354999981969158 ) ) ;
#14193 = EDGE_CURVE ( 'NONE', #2104, #15865, #18064, .T. ) ;
#14194 = EDGE_LOOP ( 'NONE', ( #14823, #6109 ) ) ;
#14195 = CARTESIAN_POINT ( 'NONE',  ( 1.084202172485504434E-14, 4.618802153517020059, -0.3572655899081733644 ) ) ;
#14196 = FACE_BOUND ( 'NONE', #5558, .T. ) ;
#14197 = CARTESIAN_POINT ( 'NONE',  ( 17.50000000000000355, -2.143131898507868643E-15, -40.00000000000000000 ) ) ;
#14198 = DIRECTION ( 'NONE',  ( 0.000000000000000000, 0.000000000000000000, -1.000000000000000000 ) ) ;
#14199 = DIRECTION ( 'NONE',  ( 1.000000000000000000, 0.000000000000000000, 0.000000000000000000 ) ) ;
#14200 = CARTESIAN_POINT ( 'NONE',  ( 10.19618095047498052, -15.25966317163203456, -3.493793749819690486 ) ) ;
#14201 = DIRECTION ( 'NONE',  ( -1.000000000000000000, 0.000000000000000000, 0.000000000000000000 ) ) ;
#14202 = VERTEX_POINT ( 'NONE', #19591 ) ;
#14203 = DIRECTION ( 'NONE',  ( 1.000000000000000000, -0.000000000000000000, -0.000000000000000000 ) ) ;
#14204 = CARTESIAN_POINT ( 'NONE',  ( 6.330490856366289165, -9.474249098604506258, -26.85745350028680534 ) ) ;
#14205 = ORIENTED_EDGE ( 'NONE', *, *, #1832, .T. ) ;
#14206 = CARTESIAN_POINT ( 'NONE',  ( 19.99999999999999645, -59.31169354540756444, 27.19476070466835438 ) ) ;
#14207 = DIRECTION ( 'NONE',  ( 0.000000000000000000, 0.000000000000000000, -1.000000000000000000 ) ) ;
#14208 = CARTESIAN_POINT ( 'NONE',  ( 0.000000000000000000, -71.89099403602357086, 3.960426305688539816 ) ) ;
#14209 = ORIENTED_EDGE ( 'NONE', *, *, #292, .T. ) ;
#14210 = CARTESIAN_POINT ( 'NONE',  ( 0.000000000000000000, 0.000000000000000000, -81.99999999999998579 ) ) ;
#14211 = VERTEX_POINT ( 'NONE', #17705 ) ;
#14212 = CARTESIAN_POINT ( 'NONE',  ( 19.99999999999999645, -54.08351995568681048, -35.76369202524558233 ) ) ;
#14213 = CARTESIAN_POINT ( 'NONE',  ( 30.00000000000000711, -30.00000000000001421, -120.0000000000000142 ) ) ;
#14214 = ORIENTED_EDGE ( 'NONE', *, *, #18820, .F. ) ;
#14215 = VERTEX_POINT ( 'NONE', #3179 ) ;
#14216 = CARTESIAN_POINT ( 'NONE',  ( 35.30716229119248339, -118.5958850092678460, -77.65589229240622160 ) ) ;
#14217 = CARTESIAN_POINT ( 'NONE',  ( 2.500000000000000000, 2.500728763858895382E-16, -2.041999999999999815 ) ) ;
#14218 = EDGE_CURVE ( 'NONE', #16683, #15235, #16016, .T. ) ;
#14219 = ADVANCED_FACE ( 'NONE', ( #14425 ), #6756, .F. ) ;
#14220 = CARTESIAN_POINT ( 'NONE',  ( 19.99999999999999645, 63.85430960833490843, 16.34407078397899227 ) ) ;
#14221 = CARTESIAN_POINT ( 'NONE',  ( -9.474249097082500626, 6.330490858644140850, -6.186296499352570422 ) ) ;
#14222 = CARTESIAN_POINT ( 'NONE',  ( 6.358192987158590270, -4.248408730893245000, -17.59260624981969201 ) ) ;
#14223 = CARTESIAN_POINT ( 'NONE',  ( 8.500000000000000000, 0.000000000000000000, 90.00000000000000000 ) ) ;
#14224 = DIRECTION ( 'NONE',  ( 0.000000000000000000, -0.8878852184023793281, 0.4600650377311439887 ) ) ;
#14225 = CARTESIAN_POINT ( 'NONE',  ( 30.00000000000000000, -39.99999999999999289, 52.00000000000000000 ) ) ;
#14226 = ORIENTED_EDGE ( 'NONE', *, *, #16875, .T. ) ;
#14227 = DIRECTION ( 'NONE',  ( -1.000000000000000000, -0.000000000000000000, -0.000000000000000000 ) ) ;
#14228 = ORIENTED_EDGE ( 'NONE', *, *, #20198, .T. ) ;
#14229 = CARTESIAN_POINT ( 'NONE',  ( -17.99999999956958519, 3.580422614997674113, -20.71401874981969016 ) ) ;
#14230 = CARTESIAN_POINT ( 'NONE',  ( 0.000000000000000000, -62.46228066917775834, -18.86519267363519958 ) ) ;
#14231 = ORIENTED_EDGE ( 'NONE', *, *, #15323, .T. ) ;
#14232 = CARTESIAN_POINT ( 'NONE',  ( -11.50000000000000000, 1.408343819019456176E-15, 68.00000000000000000 ) ) ;
#14233 = ORIENTED_EDGE ( 'NONE', *, *, #9885, .F. ) ;
#14234 = CARTESIAN_POINT ( 'NONE',  ( 6.358192987158592047, -4.248408730893246776, -8.167606249819693076 ) ) ;
#14235 = DIRECTION ( 'NONE',  ( -1.000000000000000000, 0.000000000000000000, -0.000000000000000000 ) ) ;
#14236 = CARTESIAN_POINT ( 'NONE',  ( -6.358192987158592047, 4.248408730893246776, -3.455106249819692277 ) ) ;
#14237 = AXIS2_PLACEMENT_3D ( 'NONE', #7143, #20186, #3971 ) ;
#14238 = VERTEX_POINT ( 'NONE', #9650 ) ;
#14239 = DIRECTION ( 'NONE',  ( -1.000000000000000000, 0.000000000000000000, -0.000000000000000000 ) ) ;
#14240 = CARTESIAN_POINT ( 'NONE',  ( 19.99999999999999645, -64.80702306891100761, 7.581672767546201008 ) ) ;
#14241 = CYLINDRICAL_SURFACE ( 'NONE', #18123, 10.00000000000000178 ) ;
#14242 = CYLINDRICAL_SURFACE ( 'NONE', #17076, 35.00000000000000000 ) ;
#14243 = AXIS2_PLACEMENT_3D ( 'NONE', #6288, #11475, #19228 ) ;
#14244 = DIRECTION ( 'NONE',  ( 1.000000000000000000, 0.000000000000000000, 0.000000000000000000 ) ) ;
#14245 = VERTEX_POINT ( 'NONE', #3471 ) ;
#14246 = CARTESIAN_POINT ( 'NONE',  ( -0.6554360035617894376, 4.240386000424038571, -0.1586754815284913411 ) ) ;
#14247 = DIRECTION ( 'NONE',  ( 1.000000000000000000, 0.000000000000000000, 0.000000000000000000 ) ) ;
#14248 = VECTOR ( 'NONE', #17621, 1000.000000000000000 ) ;
#14249 = ORIENTED_EDGE ( 'NONE', *, *, #3531, .F. ) ;
#14250 = EDGE_CURVE ( 'NONE', #20337, #14343, #17385, .T. ) ;
#14251 = FACE_OUTER_BOUND ( 'NONE', #15198, .T. ) ;
#14252 = CARTESIAN_POINT ( 'NONE',  ( -7.500000000000009770, 9.706494115329868228E-15, -7.498799999997683763 ) ) ;
#14253 = EDGE_CURVE ( 'NONE', #11718, #20455, #1482, .T. ) ;
#14254 = EDGE_LOOP ( 'NONE', ( #4319, #16645, #171, #7437 ) ) ;
#14255 = CARTESIAN_POINT ( 'NONE',  ( -2.163827323447878234E-09, -18.00000000000000000, -12.03519999981969235 ) ) ;
#14256 = LINE ( 'NONE', #17554, #12759 ) ;
#14257 = CARTESIAN_POINT ( 'NONE',  ( 30.00000000000000000, -122.0000000000000000, -2.100000000000004086 ) ) ;
#14258 = ORIENTED_EDGE ( 'NONE', *, *, #934, .T. ) ;
#14259 = DIRECTION ( 'NONE',  ( -1.000000000000000000, 0.000000000000000000, 0.000000000000000000 ) ) ;
#14260 = VERTEX_POINT ( 'NONE', #1795 ) ;
#14261 = DIRECTION ( 'NONE',  ( 0.000000000000000000, 0.000000000000000000, 1.000000000000000000 ) ) ;
#14262 = ADVANCED_BREP_SHAPE_REPRESENTATION ( '', ( #10589, #12461 ), #12750 ) ;
#14263 = VERTEX_POINT ( 'NONE', #8251 ) ;
#14264 = EDGE_CURVE ( 'NONE', #15500, #13708, #9257, .T. ) ;
#14265 = AXIS2_PLACEMENT_3D ( 'NONE', #6578, #18030, #16431 ) ;
#14266 = PLANE ( 'NONE',  #7703 ) ;
#14267 = CARTESIAN_POINT ( 'NONE',  ( 19.99999999999999645, 51.43306257653197378, -40.15061736769512635 ) ) ;
#14268 = CARTESIAN_POINT ( 'NONE',  ( -5.663308646854337880, 13.67243654778935991, -15.48002058115845792 ) ) ;
#14269 = VERTEX_POINT ( 'NONE', #96 ) ;
#14270 = CARTESIAN_POINT ( 'NONE',  ( -1.491842756249031954, -7.499999999820663454, -15.82541874981969698 ) ) ;
#14271 = CARTESIAN_POINT ( 'NONE',  ( 0.000000000000000000, 58.44960523466241398, -28.06621538408611016 ) ) ;
#14272 = VERTEX_POINT ( 'NONE', #20869 ) ;
#14273 = CIRCLE ( 'NONE', #11546, 72.00000000007199219 ) ;
#14274 = CARTESIAN_POINT ( 'NONE',  ( 7.653695106945543891, -20.10381028312655971, 76.71523333892115204 ) ) ;
#14275 = EDGE_CURVE ( 'NONE', #10180, #5437, #450, .T. ) ;
#14276 = CIRCLE ( 'NONE', #5117, 65.24900000006525147 ) ;
#14277 = EDGE_CURVE ( 'NONE', #12734, #10607, #1140, .T. ) ;
#14278 = DIRECTION ( 'NONE',  ( -1.000000000000000000, -0.000000000000000000, 0.000000000000000000 ) ) ;
#14279 = CARTESIAN_POINT ( 'NONE',  ( 19.99999999999999645, -71.89099403602357086, 3.960426305688543369 ) ) ;
#14280 = ORIENTED_EDGE ( 'NONE', *, *, #11299, .F. ) ;
#14281 = EDGE_CURVE ( 'NONE', #6859, #788, #6355, .T. ) ;
#14282 = EDGE_CURVE ( 'NONE', #15394, #6717, #15903, .T. ) ;
#14283 = CARTESIAN_POINT ( 'NONE',  ( 6.249999999999902300, -10.82531754730554496, -40.00000000000000000 ) ) ;
#14284 = CARTESIAN_POINT ( 'NONE',  ( 19.99999999999999645, 11.98658579560678206, -64.13855129306456604 ) ) ;
#14285 = AXIS2_PLACEMENT_3D ( 'NONE', #4029, #867, #1085 ) ;
#14286 = ORIENTED_EDGE ( 'NONE', *, *, #12634, .F. ) ;
#14287 = CYLINDRICAL_SURFACE ( 'NONE', #1790, 23.00000000000000000 ) ;
#14288 = CARTESIAN_POINT ( 'NONE',  ( -31.75000000000000000, 0.000000000000000000, 0.000000000000000000 ) ) ;
#14289 = CARTESIAN_POINT ( 'NONE',  ( 15.25966317163202568, 10.19618095047498230, -7.754643749819691401 ) ) ;
#14290 = ORIENTED_EDGE ( 'NONE', *, *, #1222, .F. ) ;
#14291 = DIRECTION ( 'NONE',  ( -0.000000000000000000, -0.000000000000000000, 1.000000000000000000 ) ) ;
#14292 = CIRCLE ( 'NONE', #19681, 2.041999999999999815 ) ;
#14293 = AXIS2_PLACEMENT_3D ( 'NONE', #10738, #12529, #13812 ) ;
#14294 = FILL_AREA_STYLE_COLOUR ( '', #10214 ) ;
#14295 = CARTESIAN_POINT ( 'NONE',  ( 30.00000000000000000, -164.9999999999999716, -50.00000000000002132 ) ) ;
#14296 = DIRECTION ( 'NONE',  ( -0.000000000000000000, 1.471414886128461471E-15, 1.000000000000000000 ) ) ;
#14297 = AXIS2_PLACEMENT_3D ( 'NONE', #5934, #18652, #17388 ) ;
#14298 = DIRECTION ( 'NONE',  ( 0.9237280213470682178, 0.3830490080632377725, 1.131240564625405124E-16 ) ) ;
#14299 = ADVANCED_FACE ( 'NONE', ( #17580 ), #17679, .T. ) ;
#14300 = CARTESIAN_POINT ( 'NONE',  ( -10.19618095047498230, 15.25966317163203279, 10.64370625018030836 ) ) ;
#14301 = EDGE_CURVE ( 'NONE', #12434, #18682, #11108, .T. ) ;
#14302 = CARTESIAN_POINT ( 'NONE',  ( -65.00002539999999840, 0.000000000000000000, 0.000000000000000000 ) ) ;
#14303 = VERTEX_POINT ( 'NONE', #12815 ) ;
#14304 = CARTESIAN_POINT ( 'NONE',  ( -27.96694501150314593, -24.74873734152930993, -130.0000000000000000 ) ) ;
#14305 = CARTESIAN_POINT ( 'NONE',  ( 4.276731812588566939, -10.32494394809438809, -26.56292225028680676 ) ) ;
#14306 = ADVANCED_FACE ( 'NONE', ( #6630 ), #3151, .T. ) ;
#14307 = FACE_OUTER_BOUND ( 'NONE', #854, .T. ) ;
#14308 = AXIS2_PLACEMENT_3D ( 'NONE', #10268, #9678, #4793 ) ;
#14309 = VECTOR ( 'NONE', #13157, 1000.000000000000000 ) ;
#14310 = ORIENTED_EDGE ( 'NONE', *, *, #13593, .F. ) ;
#14311 = AXIS2_PLACEMENT_3D ( 'NONE', #18302, #10463, #508 ) ;
#14312 = PLANE ( 'NONE',  #4842 ) ;
#14313 = FACE_BOUND ( 'NONE', #1965, .T. ) ;
#14314 = DIRECTION ( 'NONE',  ( 0.000000000000000000, 0.000000000000000000, -1.000000000000000000 ) ) ;
#14315 = AXIS2_PLACEMENT_3D ( 'NONE', #10574, #12264, #15341 ) ;
#14316 = EDGE_LOOP ( 'NONE', ( #8557, #9704, #5403, #20757 ) ) ;
#14317 = DIRECTION ( 'NONE',  ( 0.5000000000000066613, 0.8660254037844348218, -0.000000000000000000 ) ) ;
#14318 = EDGE_LOOP ( 'NONE', ( #8843, #5479, #3986, #16382 ) ) ;
#14319 = DIRECTION ( 'NONE',  ( 0.000000000000000000, -0.8169698930104354329, -0.5766803221148764091 ) ) ;
#14320 = PLANE ( 'NONE',  #20756 ) ;
#14321 = ORIENTED_EDGE ( 'NONE', *, *, #11876, .T. ) ;
#14322 = CIRCLE ( 'NONE', #18763, 10.79377999999999993 ) ;
#14323 = ORIENTED_EDGE ( 'NONE', *, *, #2649, .T. ) ;
#14324 = CARTESIAN_POINT ( 'NONE',  ( 50.00000000000000000, 31.35083268962916137, 50.63110039191614220 ) ) ;
#14325 =( NAMED_UNIT ( * ) PLANE_ANGLE_UNIT ( ) SI_UNIT ( $, .RADIAN. ) );
#14326 = CYLINDRICAL_SURFACE ( 'NONE', #8560, 27.60000000002760245 ) ;
#14327 = AXIS2_PLACEMENT_3D ( 'NONE', #5560, #18512, #18613 ) ;
#14328 = AXIS2_PLACEMENT_3D ( 'NONE', #1887, #15209, #2497 ) ;
#14329 = AXIS2_PLACEMENT_3D ( 'NONE', #11031, #10730, #15901 ) ;
#14330 = CARTESIAN_POINT ( 'NONE',  ( 0.000000000000000000, 2.357898499370433054, -1.951563910473907981E-15 ) ) ;
#14331 = CARTESIAN_POINT ( 'NONE',  ( -9.474249097082500626, 6.330490858644140850, -15.61129649935257646 ) ) ;
#14332 = CARTESIAN_POINT ( 'NONE',  ( -6.330490856366290053, 9.474249098604506258, 15.55504649971320141 ) ) ;
#14333 = CARTESIAN_POINT ( 'NONE',  ( -24.99999999999999289, -159.9999999999999716, 85.00000000000000000 ) ) ;
#14334 = VECTOR ( 'NONE', #7454, 1000.000000000000000 ) ;
#14335 = DIRECTION ( 'NONE',  ( -0.000000000000000000, -0.000000000000000000, 1.000000000000000000 ) ) ;
#14336 = CYLINDRICAL_SURFACE ( 'NONE', #12038, 7.500000000000000000 ) ;
#14337 = VERTEX_POINT ( 'NONE', #1575 ) ;
#14338 = DIRECTION ( 'NONE',  ( -1.000000000000000000, 0.000000000000000000, 0.000000000000000000 ) ) ;
#14339 = ORIENTED_EDGE ( 'NONE', *, *, #15063, .F. ) ;
#14340 = CARTESIAN_POINT ( 'NONE',  ( -2.163827323447878234E-09, -18.00000000000000000, -13.93979999981969087 ) ) ;
#14341 = DIRECTION ( 'NONE',  ( 0.000000000000000000, 0.000000000000000000, 1.000000000000000000 ) ) ;
#14342 = VECTOR ( 'NONE', #9899, 1000.000000000000000 ) ;
#14343 = VERTEX_POINT ( 'NONE', #14508 ) ;
#14344 = CIRCLE ( 'NONE', #6201, 10.85999999999999410 ) ;
#14345 = CARTESIAN_POINT ( 'NONE',  ( -6.359999999999995879, -10.52399999999999025, 1.288818291422673979E-15 ) ) ;
#14346 = ORIENTED_EDGE ( 'NONE', *, *, #18258, .F. ) ;
#14347 = FACE_BOUND ( 'NONE', #9290, .T. ) ;
#14348 = FACE_OUTER_BOUND ( 'NONE', #3368, .T. ) ;
#14349 = CARTESIAN_POINT ( 'NONE',  ( 5.303300859536631329, 5.303300858261585482, -0.8043249998196909667 ) ) ;
#14350 = ADVANCED_FACE ( 'NONE', ( #9509, #14400 ), #7922, .T. ) ;
#14351 = EDGE_CURVE ( 'NONE', #18356, #14556, #13656, .T. ) ;
#14352 = VERTEX_POINT ( 'NONE', #17889 ) ;
#14353 = LINE ( 'NONE', #9561, #7292 ) ;
#14354 = CIRCLE ( 'NONE', #16036, 14.49999999999999822 ) ;
#14355 = DIRECTION ( 'NONE',  ( -1.000000000000000000, 0.000000000000000000, 0.000000000000000000 ) ) ;
#14356 = DIRECTION ( 'NONE',  ( 0.000000000000000000, 0.000000000000000000, 1.000000000000000000 ) ) ;
#14357 = CIRCLE ( 'NONE', #16702, 7.500000000000000000 ) ;
#14358 = CYLINDRICAL_SURFACE ( 'NONE', #19089, 39.99999999999999289 ) ;
#14360 = ORIENTED_EDGE ( 'NONE', *, *, #17779, .T. ) ;
#14359 = AXIS2_PLACEMENT_3D ( 'NONE', #5606, #7194, #20015 ) ;
#14361 = LINE ( 'NONE', #12775, #529 ) ;
#14362 = DIRECTION ( 'NONE',  ( -1.000000000000000000, -0.000000000000000000, -0.000000000000000000 ) ) ;
#14363 = EDGE_LOOP ( 'NONE', ( #991, #10099, #6586, #10988 ) ) ;
#14364 = CARTESIAN_POINT ( 'NONE',  ( 19.74873734152915716, 24.74873734152916072, -120.0000000000000142 ) ) ;
#14365 = FACE_OUTER_BOUND ( 'NONE', #17321, .T. ) ;
#14366 = EDGE_LOOP ( 'NONE', ( #10358, #16954, #3683, #19217 ) ) ;
#14367 = DIRECTION ( 'NONE',  ( 0.000000000000000000, 0.000000000000000000, -1.000000000000000000 ) ) ;
#14368 = FACE_OUTER_BOUND ( 'NONE', #20692, .T. ) ;
#14369 = DIRECTION ( 'NONE',  ( -0.000000000000000000, -0.000000000000000000, -1.000000000000000000 ) ) ;
#14370 = AXIS2_PLACEMENT_3D ( 'NONE', #3927, #13696, #8488 ) ;
#14371 = ORIENTED_EDGE ( 'NONE', *, *, #8305, .T. ) ;
#14372 = CIRCLE ( 'NONE', #18403, 65.24900000006525147 ) ;
#14373 = CARTESIAN_POINT ( 'NONE',  ( 19.99999999999999645, 0.000000000000000000, 0.000000000000000000 ) ) ;
#14374 = VERTEX_POINT ( 'NONE', #1474 ) ;
#14375 = CARTESIAN_POINT ( 'NONE',  ( 0.000000000000000000, -29.55812890831937878, -65.65300461859717984 ) ) ;
#14376 = EDGE_CURVE ( 'NONE', #9288, #10742, #19079, .T. ) ;
#14377 = ORIENTED_EDGE ( 'NONE', *, *, #16263, .T. ) ;
#14378 = VECTOR ( 'NONE', #9992, 1000.000000000000000 ) ;
#14379 = CYLINDRICAL_SURFACE ( 'NONE', #15824, 27.60000000002760245 ) ;
#14380 = EDGE_CURVE ( 'NONE', #7721, #1433, #8725, .T. ) ;
#14381 = FACE_OUTER_BOUND ( 'NONE', #6135, .T. ) ;
#14382 = CONTEXT_DEPENDENT_SHAPE_REPRESENTATION ( #9931, #20152 ) ;
#14383 = VECTOR ( 'NONE', #9566, 1000.000000000000000 ) ;
#14384 = CARTESIAN_POINT ( 'NONE',  ( 10.32494394809439875, 4.276731812588567827, 25.32854725064742851 ) ) ;
#14385 = ORIENTED_EDGE ( 'NONE', *, *, #16550, .T. ) ;
#14386 = DIRECTION ( 'NONE',  ( -1.648349939164583742E-16, 1.000000000000000000, 0.000000000000000000 ) ) ;
#14387 = FACE_BOUND ( 'NONE', #3860, .T. ) ;
#14388 = ORIENTED_EDGE ( 'NONE', *, *, #5358, .T. ) ;
#14389 = CARTESIAN_POINT ( 'NONE',  ( -6.358192988180015881, -4.248408729364577141, -24.07229374981969627 ) ) ;
#14390 = DIRECTION ( 'NONE',  ( 0.000000000000000000, 0.000000000000000000, 1.000000000000000000 ) ) ;
#14391 = CARTESIAN_POINT ( 'NONE',  ( 17.00000000000000000, 0.000000000000000000, 0.000000000000000000 ) ) ;
#14392 = ORIENTED_EDGE ( 'NONE', *, *, #7956, .F. ) ;
#14393 = DIRECTION ( 'NONE',  ( -0.000000000000000000, -0.000000000000000000, 1.000000000000000000 ) ) ;
#14394 = DIRECTION ( 'NONE',  ( 0.000000000000000000, 0.000000000000000000, 1.000000000000000000 ) ) ;
#14395 = PRESENTATION_LAYER_ASSIGNMENT (  '', '', ( #4227 ) ) ;
#14396 = ORIENTED_EDGE ( 'NONE', *, *, #210, .F. ) ;
#14397 = CARTESIAN_POINT ( 'NONE',  ( -10.27973195343232149, -20.58856569599344510, -76.47391966369774252 ) ) ;
#14398 = VECTOR ( 'NONE', #9662, 1000.000000000000000 ) ;
#14399 = CARTESIAN_POINT ( 'NONE',  ( 19.99999999999999645, 64.79224928664392280, -2.456263514197840614 ) ) ;
#14400 = FACE_BOUND ( 'NONE', #7034, .T. ) ;
#14401 = VERTEX_POINT ( 'NONE', #20499 ) ;
#14402 = DIRECTION ( 'NONE',  ( 0.000000000000000000, 0.000000000000000000, 1.000000000000000000 ) ) ;
#14403 = ADVANCED_FACE ( 'NONE', ( #14157, #14365 ), #3014, .F. ) ;
#14404 = FACE_OUTER_BOUND ( 'NONE', #8903, .T. ) ;
#14405 = ADVANCED_FACE ( 'NONE', ( #2696 ), #18813, .F. ) ;
#14406 = FACE_OUTER_BOUND ( 'NONE', #6441, .T. ) ;
#14407 = DIRECTION ( 'NONE',  ( 0.000000000000000000, 0.000000000000000000, 1.000000000000000000 ) ) ;
#14408 = CARTESIAN_POINT ( 'NONE',  ( -3.580422614997675890, -17.99999999956958519, -21.16566874981969093 ) ) ;
#14409 = LINE ( 'NONE', #6339, #7911 ) ;
#14410 = EDGE_CURVE ( 'NONE', #6625, #3107, #12984, .T. ) ;
#14411 = EDGE_LOOP ( 'NONE', ( #4408, #8061 ) ) ;
#14412 = CARTESIAN_POINT ( 'NONE',  ( -21.45900938229203447, -1.326995226329880762, -84.99999999999998579 ) ) ;
#14413 = CARTESIAN_POINT ( 'NONE',  ( 13.67243654642774686, -5.663308650141536837, -8.138729418480927791 ) ) ;
#14414 = FACE_OUTER_BOUND ( 'NONE', #7733, .T. ) ;
#14415 = CIRCLE ( 'NONE', #6280, 72.00000000007199219 ) ;
#14416 = VERTEX_POINT ( 'NONE', #14051 ) ;
#14417 = DIRECTION ( 'NONE',  ( -1.000000000000000000, 0.000000000000000000, -0.000000000000000000 ) ) ;
#14418 = CARTESIAN_POINT ( 'NONE',  ( 2.500000000000000000, 2.357898499370433054, -1.951563910473907981E-15 ) ) ;
#14419 = CARTESIAN_POINT ( 'NONE',  ( 19.99999999999999645, -18.50424539729796791, -69.58155576219134275 ) ) ;
#14420 = EDGE_LOOP ( 'NONE', ( #1895, #11714 ) ) ;
#14421 = EDGE_CURVE ( 'NONE', #6083, #13598, #2801, .T. ) ;
#14422 = DIRECTION ( 'NONE',  ( 0.000000000000000000, 0.000000000000000000, 1.000000000000000000 ) ) ;
#14423 = EDGE_LOOP ( 'NONE', ( #18191, #9738 ) ) ;
#14424 = CARTESIAN_POINT ( 'NONE',  ( 24.99999999999999645, -85.00000000000000000, -1.040949779275250179E-14 ) ) ;
#14425 = FACE_OUTER_BOUND ( 'NONE', #12298, .T. ) ;
#14426 = EDGE_LOOP ( 'NONE', ( #4291, #18999, #10721, #11605 ) ) ;
#14427 = ORIENTED_EDGE ( 'NONE', *, *, #17922, .F. ) ;
#14428 = CARTESIAN_POINT ( 'NONE',  ( 50.00000000000000000, -42.57363661491096707, -121.3828884801879155 ) ) ;
#14429 = EDGE_CURVE ( 'NONE', #16465, #13160, #17113, .T. ) ;
#14430 = CIRCLE ( 'NONE', #10702, 10.52399999999999380 ) ;
#14431 = EDGE_CURVE ( 'NONE', #6278, #833, #9922, .T. ) ;
#14432 = LINE ( 'NONE', #6561, #13672 ) ;
#14433 = AXIS2_PLACEMENT_3D ( 'NONE', #19605, #5081, #12849 ) ;
#14434 = ADVANCED_FACE ( 'NONE', ( #9160 ), #18921, .T. ) ;
#14435 = CARTESIAN_POINT ( 'NONE',  ( 62.49999999999999289, -30.00000000000000000, 0.000000000000000000 ) ) ;
#14436 = CARTESIAN_POINT ( 'NONE',  ( 2.222972771497741640, 11.17563879704982988, -4.419108999352573619 ) ) ;
#14437 = CARTESIAN_POINT ( 'NONE',  ( 6.929096494179676213, 2.870125741905210415, -19.06526249981969201 ) ) ;
#14438 = CARTESIAN_POINT ( 'NONE',  ( 0.000000000000000000, 3.141410481201071914, 65.17333458706188765 ) ) ;
#14439 = CARTESIAN_POINT ( 'NONE',  ( 19.99999999999999645, 3.141410481201988070, -65.17333458706183080 ) ) ;
#14440 = CARTESIAN_POINT ( 'NONE',  ( 0.000000000000000000, -63.05226888949880504, -15.11556105343524514 ) ) ;
#14441 = MECHANICAL_DESIGN_GEOMETRIC_PRESENTATION_REPRESENTATION (  '', ( #7959 ), #14758 ) ;
#14442 = ORIENTED_EDGE ( 'NONE', *, *, #2705, .F. ) ;
#14443 = FACE_OUTER_BOUND ( 'NONE', #13719, .T. ) ;
#14444 = CIRCLE ( 'NONE', #15109, 27.60000000002760245 ) ;
#14445 = ORIENTED_EDGE ( 'NONE', *, *, #9340, .T. ) ;
#14446 = CARTESIAN_POINT ( 'NONE',  ( 16.62983158603122291, 6.888301780572502864, -16.88511249981969087 ) ) ;
#14447 = DIRECTION ( 'NONE',  ( -1.000000000000000000, 0.000000000000000000, -0.000000000000000000 ) ) ;
#14448 = ORIENTED_EDGE ( 'NONE', *, *, #14282, .F. ) ;
#14449 = EDGE_CURVE ( 'NONE', #11681, #1468, #12453, .T. ) ;
#14450 = FACE_OUTER_BOUND ( 'NONE', #13941, .T. ) ;
#14451 = AXIS2_PLACEMENT_3D ( 'NONE', #11276, #2806, #7571 ) ;
#14452 = EDGE_LOOP ( 'NONE', ( #15274, #2525, #4436, #15139 ) ) ;
#14453 = AXIS2_PLACEMENT_3D ( 'NONE', #6415, #6008, #14184 ) ;
#14454 = CARTESIAN_POINT ( 'NONE',  ( 19.99999999999999645, -58.26603306961934692, -42.29739224042532442 ) ) ;
#14455 = FACE_OUTER_BOUND ( 'NONE', #270, .T. ) ;
#14456 = CARTESIAN_POINT ( 'NONE',  ( 0.000000000000000000, -59.36728637277992249, -40.73727173906846843 ) ) ;
#14457 = EDGE_LOOP ( 'NONE', ( #7371, #15868, #19817, #11207 ) ) ;
#14458 = FACE_BOUND ( 'NONE', #13500, .T. ) ;
#14459 = EDGE_CURVE ( 'NONE', #12652, #10139, #17549, .T. ) ;
#14460 = AXIS2_PLACEMENT_3D ( 'NONE', #3068, #6140, #13891 ) ;
#14461 = CARTESIAN_POINT ( 'NONE',  ( -62.49999999999999289, -30.00000000000000000, 5.000000000000000000 ) ) ;
#14462 = DIRECTION ( 'NONE',  ( -1.000000000000000000, 0.000000000000000000, -0.000000000000000000 ) ) ;
#14463 = AXIS2_PLACEMENT_3D ( 'NONE', #9950, #205, #16615 ) ;
#14464 = VECTOR ( 'NONE', #20766, 1000.000000000000000 ) ;
#14465 = DIRECTION ( 'NONE',  ( -0.000000000000000000, 0.000000000000000000, 1.000000000000000000 ) ) ;
#14466 = ORIENTED_EDGE ( 'NONE', *, *, #13864, .F. ) ;
#14467 = DIRECTION ( 'NONE',  ( 0.000000000000000000, -0.5000000000000009992, -0.8660254037844380415 ) ) ;
#14468 = EDGE_CURVE ( 'NONE', #9747, #15390, #12554, .T. ) ;
#14469 =( GEOMETRIC_REPRESENTATION_CONTEXT ( 3 ) GLOBAL_UNCERTAINTY_ASSIGNED_CONTEXT ( ( #4337 ) ) GLOBAL_UNIT_ASSIGNED_CONTEXT ( ( #4024, #3920, #10404 ) ) REPRESENTATION_CONTEXT ( 'NONE', 'WORKASPACE' ) );
#14470 = CARTESIAN_POINT ( 'NONE',  ( 19.99999999999999645, -3.141410481200616278, -65.17333458706190186 ) ) ;
#14471 = ORIENTED_EDGE ( 'NONE', *, *, #730, .T. ) ;
#14472 = CARTESIAN_POINT ( 'NONE',  ( 19.99999999999999645, 42.42902769288603082, -49.02903636734153281 ) ) ;
#14473 = CARTESIAN_POINT ( 'NONE',  ( 19.99999999999999645, -60.35829202194891252, 24.78524934717529504 ) ) ;
#14474 = ORIENTED_EDGE ( 'NONE', *, *, #381, .F. ) ;
#14475 = CARTESIAN_POINT ( 'NONE',  ( -52.00000000000000000, -99.99999999999998579, 5.000000000000000000 ) ) ;
#14476 = DIRECTION ( 'NONE',  ( 0.000000000000000000, 0.6310879443260485333, 0.7757112907044232397 ) ) ;
#14477 = DIRECTION ( 'NONE',  ( -1.000000000000000000, -0.000000000000000000, -0.000000000000000000 ) ) ;
#14478 = AXIS2_PLACEMENT_3D ( 'NONE', #3800, #10284, #10390 ) ;
#14479 = EDGE_LOOP ( 'NONE', ( #4814, #11131, #9930, #1800, #18154, #2853, #2190, #20399, #15880, #18043, #13521, #3509, #20204 ) ) ;
#14480 = LINE ( 'NONE', #9892, #10616 ) ;
#14481 = ORIENTED_EDGE ( 'NONE', *, *, #7927, .T. ) ;
#14482 = DIRECTION ( 'NONE',  ( -1.000000000000000000, 0.000000000000000000, 0.000000000000000000 ) ) ;
#14483 = CIRCLE ( 'NONE', #3943, 21.50000000000000000 ) ;
#14484 = ORIENTED_EDGE ( 'NONE', *, *, #1646, .F. ) ;
#14485 = AXIS2_PLACEMENT_3D ( 'NONE', #8020, #15566, #14500 ) ;
#14486 = CARTESIAN_POINT ( 'NONE',  ( 39.99999999999997158, -122.3205080756887497, -80.28096411455980785 ) ) ;
#14487 = CARTESIAN_POINT ( 'NONE',  ( -26.35784117651625280, 26.35784117651607872, -120.0000000000000142 ) ) ;
#14488 = AXIS2_PLACEMENT_3D ( 'NONE', #5786, #18846, #15760 ) ;
#14489 = CARTESIAN_POINT ( 'NONE',  ( -12.54593441764187745, -8.382925368423274293, -18.13080183115846111 ) ) ;
#14490 = EDGE_CURVE ( 'NONE', #10560, #17270, #1119, .T. ) ;
#14491 = VERTEX_POINT ( 'NONE', #1229 ) ;
#14492 = CARTESIAN_POINT ( 'NONE',  ( 5.303300858261583706, -5.303300859536632217, -17.29807499981969343 ) ) ;
#14493 = EDGE_CURVE ( 'NONE', #19457, #17375, #4387, .T. ) ;
#14494 = VECTOR ( 'NONE', #13949, 1000.000000000000000 ) ;
#14495 = DIRECTION ( 'NONE',  ( -1.000000000000000000, 0.000000000000000000, -0.000000000000000000 ) ) ;
#14496 = VERTEX_POINT ( 'NONE', #9270 ) ;
#14497 = CARTESIAN_POINT ( 'NONE',  ( -24.99999999999999289, -42.57363661491096707, 121.3828884801879155 ) ) ;
#14498 = AXIS2_PLACEMENT_3D ( 'NONE', #19878, #15006, #6276 ) ;
#14499 = DIRECTION ( 'NONE',  ( 1.000000000000000000, 0.000000000000000000, 0.000000000000000000 ) ) ;
#14500 = DIRECTION ( 'NONE',  ( -1.000000000000000000, 0.000000000000000000, 0.000000000000000000 ) ) ;
#14501 = DIRECTION ( 'NONE',  ( 0.000000000000000000, 0.6310879443260485333, 0.7757112907044232397 ) ) ;
#14502 = VERTEX_POINT ( 'NONE', #5875 ) ;
#14503 = CARTESIAN_POINT ( 'NONE',  ( -49.35000000000000142, -99.99999999999998579, 5.000000000000000000 ) ) ;
#14504 = DIRECTION ( 'NONE',  ( 0.000000000000000000, -1.000000000000000000, 1.224646799147355426E-16 ) ) ;
#14505 = EDGE_LOOP ( 'NONE', ( #343, #13657 ) ) ;
#14506 = CARTESIAN_POINT ( 'NONE',  ( -13.44994733502084294, -18.67183681267612982, -77.46342352758064465 ) ) ;
#14507 = DIRECTION ( 'NONE',  ( 1.000000000000000000, -0.000000000000000000, 0.000000000000000000 ) ) ;
#14508 = CARTESIAN_POINT ( 'NONE',  ( 29.74873734152916782, 24.74873734152916072, -130.0000000000000000 ) ) ;
#14509 = ORIENTED_EDGE ( 'NONE', *, *, #769, .T. ) ;
#14510 = FACE_OUTER_BOUND ( 'NONE', #676, .T. ) ;
#14511 = CARTESIAN_POINT ( 'NONE',  ( 9.999999999999998224, -70.68211945903179583, -13.71269443944282607 ) ) ;
#14512 = DIRECTION ( 'NONE',  ( 3.374236624099838250E-32, -1.836909530733573776E-16, 1.000000000000000000 ) ) ;
#14513 = CARTESIAN_POINT ( 'NONE',  ( 10.19618095047498052, -15.25966317163203456, -22.34379374981969235 ) ) ;
#14514 = EDGE_LOOP ( 'NONE', ( #16507, #13111, #16521, #6544 ) ) ;
#14515 = CARTESIAN_POINT ( 'NONE',  ( 85.00002539999999840, 9.184850993605147944E-16, -7.500000000000000000 ) ) ;
#14516 = CARTESIAN_POINT ( 'NONE',  ( 19.99999999999999645, 0.000000000000000000, 0.000000000000000000 ) ) ;
#14517 = CARTESIAN_POINT ( 'NONE',  ( -14.79893867722910095, 2.943691928843434891, -3.720760668480927347 ) ) ;
#14518 = DIRECTION ( 'NONE',  ( -0.000000000000000000, -0.000000000000000000, 1.000000000000000000 ) ) ;
#14519 = EDGE_CURVE ( 'NONE', #15789, #8899, #17027, .T. ) ;
#14520 = ORIENTED_EDGE ( 'NONE', *, *, #5463, .F. ) ;
#14521 = LINE ( 'NONE', #8620, #13989 ) ;
#14522 = CARTESIAN_POINT ( 'NONE',  ( -5.303300858261589035, 5.303300859536635770, 21.95432500018031874 ) ) ;
#14523 = DIRECTION ( 'NONE',  ( 1.000000000000000000, -0.000000000000000000, -0.000000000000000000 ) ) ;
#14524 = VERTEX_POINT ( 'NONE', #15840 ) ;
#14525 = CARTESIAN_POINT ( 'NONE',  ( 30.00000000000000000, -39.99999999999999289, -52.00000000000000000 ) ) ;
#14526 = EDGE_LOOP ( 'NONE', ( #16512, #7275, #18798, #201, #3015, #11698 ) ) ;
#14527 = CARTESIAN_POINT ( 'NONE',  ( 19.99999999999999645, 64.79224928664392280, -2.456263514197840614 ) ) ;
#14528 = CARTESIAN_POINT ( 'NONE',  ( 9.999999999999998224, -36.59093685910671212, 62.00889726308019334 ) ) ;
#14529 = VERTEX_POINT ( 'NONE', #20698 ) ;
#14530 = EDGE_CURVE ( 'NONE', #15865, #8953, #6219, .T. ) ;
#14531 = ORIENTED_EDGE ( 'NONE', *, *, #366, .T. ) ;
#14532 = CARTESIAN_POINT ( 'NONE',  ( 19.99999999999999645, 0.000000000000000000, 0.000000000000000000 ) ) ;
#14533 = EDGE_CURVE ( 'NONE', #4467, #10293, #19098, .T. ) ;
#14534 = FILL_AREA_STYLE ('',( #1508 ) ) ;
#14535 = FACE_OUTER_BOUND ( 'NONE', #16585, .T. ) ;
#14536 = DIRECTION ( 'NONE',  ( -0.000000000000000000, -0.000000000000000000, -1.000000000000000000 ) ) ;
#14537 = CARTESIAN_POINT ( 'NONE',  ( 6.929096494179683319, 2.870125741905213079, 15.47463750018031625 ) ) ;
#14538 = CARTESIAN_POINT ( 'NONE',  ( 2.222972768810837163, -11.17563879758427525, 2.006608999713197949 ) ) ;
#14539 = FACE_OUTER_BOUND ( 'NONE', #10335, .T. ) ;
#14540 = CYLINDRICAL_SURFACE ( 'NONE', #10847, 65.24900000006525147 ) ;
#14541 = DIRECTION ( 'NONE',  ( 1.000000000000000000, 0.000000000000000000, 0.000000000000000000 ) ) ;
#14542 = EDGE_CURVE ( 'NONE', #17883, #19366, #16451, .T. ) ;
#14543 = ORIENTED_EDGE ( 'NONE', *, *, #15687, .T. ) ;
#14544 = DIRECTION ( 'NONE',  ( -0.000000000000000000, -0.000000000000000000, -1.000000000000000000 ) ) ;
#14545 = EDGE_CURVE ( 'NONE', #12799, #15624, #11633, .T. ) ;
#14546 = ORIENTED_EDGE ( 'NONE', *, *, #18207, .F. ) ;
#14547 = CARTESIAN_POINT ( 'NONE',  ( -15.25966317163203279, -10.19618095047498052, 17.71245625018031689 ) ) ;
#14548 = LINE ( 'NONE', #1817, #5901 ) ;
#14549 = ORIENTED_EDGE ( 'NONE', *, *, #7606, .T. ) ;
#14550 = CARTESIAN_POINT ( 'NONE',  ( 19.99999999999999645, 0.000000000000000000, 0.000000000000000000 ) ) ;
#14551 = ORIENTED_EDGE ( 'NONE', *, *, #2294, .T. ) ;
#14552 = CARTESIAN_POINT ( 'NONE',  ( 54.64999999999999858, -99.99999999999998579, 5.000000000000000000 ) ) ;
#14553 = CARTESIAN_POINT ( 'NONE',  ( 37.43953707193390557, -20.06695501706099094, 76.69796010862685876 ) ) ;
#14554 = EDGE_CURVE ( 'NONE', #11249, #13182, #6547, .T. ) ;
#14555 = EDGE_LOOP ( 'NONE', ( #3658, #1236, #7174, #10960 ) ) ;
#14556 = VERTEX_POINT ( 'NONE', #14763 ) ;
#14557 = CARTESIAN_POINT ( 'NONE',  ( 0.000000000000000000, -63.48283426024875808, 33.96954156735347397 ) ) ;
#14558 = DIRECTION ( 'NONE',  ( 0.000000000000000000, 0.000000000000000000, 1.000000000000000000 ) ) ;
#14559 = DIRECTION ( 'NONE',  ( -1.000000000000000000, 0.000000000000000000, 0.000000000000000000 ) ) ;
#14560 = EDGE_CURVE ( 'NONE', #16951, #9969, #14354, .T. ) ;
#14561 = ORIENTED_EDGE ( 'NONE', *, *, #20871, .F. ) ;
#14562 = EDGE_CURVE ( 'NONE', #9460, #4144, #5528, .T. ) ;
#14563 = AXIS2_PLACEMENT_3D ( 'NONE', #15956, #6003, #20934 ) ;
#14564 = CARTESIAN_POINT ( 'NONE',  ( -2.870125741905209971, 6.929096494179676213, 6.853487500180312608 ) ) ;
#14565 = LINE ( 'NONE', #20694, #17959 ) ;
#14566 = LINE ( 'NONE', #16349, #11322 ) ;
#14567 = CARTESIAN_POINT ( 'NONE',  ( -6.177131623262581250, 10.85999999999999410, 0.000000000000000000 ) ) ;
#14568 = ORIENTED_EDGE ( 'NONE', *, *, #6253, .F. ) ;
#14569 = DIRECTION ( 'NONE',  ( -0.000000000000000000, -0.000000000000000000, 1.000000000000000000 ) ) ;
#14570 = ADVANCED_FACE ( 'NONE', ( #11576 ), #3218, .F. ) ;
#14571 = DIRECTION ( 'NONE',  ( -1.000000000000000000, 0.000000000000000000, -0.000000000000000000 ) ) ;
#14572 = CARTESIAN_POINT ( 'NONE',  ( 19.99999999999999645, -31.17893654894269773, 57.31758819669160232 ) ) ;
#14573 = VERTEX_POINT ( 'NONE', #14473 ) ;
#14574 = FACE_OUTER_BOUND ( 'NONE', #2360, .T. ) ;
#14575 = ORIENTED_EDGE ( 'NONE', *, *, #3388, .T. ) ;
#14576 = CARTESIAN_POINT ( 'NONE',  ( -52.49999999999999289, -30.00000000000000000, 5.000000000000000000 ) ) ;
#14577 = VERTEX_POINT ( 'NONE', #3516 ) ;
#14578 = AXIS2_PLACEMENT_3D ( 'NONE', #19931, #1935, #2348 ) ;
#14579 = CARTESIAN_POINT ( 'NONE',  ( 19.99999999999999645, 38.69327817041845918, -52.53819777490596010 ) ) ;
#14580 = CARTESIAN_POINT ( 'NONE',  ( 7.500000000000000000, 9.184850993605147944E-16, -40.00000000000000000 ) ) ;
#14581 = CIRCLE ( 'NONE', #20305, 27.60000000002760245 ) ;
#14582 = CARTESIAN_POINT ( 'NONE',  ( 10.46442989202484064, -10.46442989454075878, -20.78158308115845898 ) ) ;
#14583 = ORIENTED_EDGE ( 'NONE', *, *, #17373, .F. ) ;
#14584 = CARTESIAN_POINT ( 'NONE',  ( 40.00000000000000711, 29.99999999999999289, -130.0000000000000000 ) ) ;
#14585 = LINE ( 'NONE', #17876, #1798 ) ;
#14586 = ORIENTED_EDGE ( 'NONE', *, *, #294, .F. ) ;
#14587 = CARTESIAN_POINT ( 'NONE',  ( 7.500000000000000000, 9.184850993605147944E-16, 40.00000000000000000 ) ) ;
#14588 = CARTESIAN_POINT ( 'NONE',  ( 16.62983158603122291, 6.888301780572502864, 22.71948750018031404 ) ) ;
#14589 = CARTESIAN_POINT ( 'NONE',  ( -65.00002539999999840, 5.400000000000000355, -1.000000000000000000 ) ) ;
#14590 = CARTESIAN_POINT ( 'NONE',  ( 0.000000000000000000, 0.000000000000000000, 0.000000000000000000 ) ) ;
#14591 = ORIENTED_EDGE ( 'NONE', *, *, #10129, .F. ) ;
#14592 = DIRECTION ( 'NONE',  ( 0.000000000000000000, 0.000000000000000000, -1.000000000000000000 ) ) ;
#14593 = CIRCLE ( 'NONE', #4767, 10.00000000000000178 ) ;
#14594 = ORIENTED_EDGE ( 'NONE', *, *, #13269, .F. ) ;
#14595 = CYLINDRICAL_SURFACE ( 'NONE', #4134, 8.999999999999994671 ) ;
#14596 = DIRECTION ( 'NONE',  ( 1.000000000000000000, 0.000000000000000000, 0.000000000000000000 ) ) ;
#14597 = CARTESIAN_POINT ( 'NONE',  ( 2.870125743571140475, 6.929096493489632635, -4.553487499819687478 ) ) ;
#14598 = EDGE_CURVE ( 'NONE', #4487, #14705, #4181, .T. ) ;
#14599 = EDGE_LOOP ( 'NONE', ( #20938, #3444, #14619, #6942 ) ) ;
#14600 = CARTESIAN_POINT ( 'NONE',  ( 19.99999999999999645, 59.36728637278018539, 40.73727173906806343 ) ) ;
#14601 = CARTESIAN_POINT ( 'NONE',  ( 9.999999999999998224, 29.55812890831981932, 65.65300461859698089 ) ) ;
#14602 = CARTESIAN_POINT ( 'NONE',  ( 15.25966317163203101, 10.19618095047498585, -5.850043749819691996 ) ) ;
#14604 = VERTEX_POINT ( 'NONE', #8395 ) ;
#14603 = CIRCLE ( 'NONE', #18664, 2.500000000000000444 ) ;
#14605 = CARTESIAN_POINT ( 'NONE',  ( 0.000000000000000000, -63.85430960833497949, 11.25592921604817676 ) ) ;
#14606 = CIRCLE ( 'NONE', #2070, 27.60000000002760245 ) ;
#14607 = DIRECTION ( 'NONE',  ( -1.000000000000000000, 0.000000000000000000, -0.000000000000000000 ) ) ;
#14608 = CARTESIAN_POINT ( 'NONE',  ( 10.46442989454075168, 10.46442989202483886, -0.4809169184809246600 ) ) ;
#14609 = FACE_OUTER_BOUND ( 'NONE', #372, .T. ) ;
#14610 = AXIS2_PLACEMENT_3D ( 'NONE', #9446, #15906, #7852 ) ;
#14611 = B_SPLINE_CURVE_WITH_KNOTS ( 'NONE', 3,
 ( #20053, #8819, #2164, #7344 ),
 .UNSPECIFIED., .F., .F.,
 ( 4, 4 ),
 ( 6.938893903907228378E-18, 0.007425583459339141733 ),
 .UNSPECIFIED. ) ;
#14612 = EDGE_LOOP ( 'NONE', ( #19759, #16256, #19540, #3707 ) ) ;
#14613 = FACE_OUTER_BOUND ( 'NONE', #19945, .T. ) ;
#14614 = CARTESIAN_POINT ( 'NONE',  ( -15.15000000000000036, 3.245314017740477087E-16, 43.00000000000000000 ) ) ;
#14615 = LINE ( 'NONE', #91, #15821 ) ;
#14616 = VERTEX_POINT ( 'NONE', #6700 ) ;
#14617 = LINE ( 'NONE', #19380, #756 ) ;
#14618 = AXIS2_PLACEMENT_3D ( 'NONE', #12878, #19323, #11274 ) ;
#14619 = ORIENTED_EDGE ( 'NONE', *, *, #5507, .T. ) ;
#14620 = DIRECTION ( 'NONE',  ( 0.000000000000000000, 0.000000000000000000, -1.000000000000000000 ) ) ;
#14621 = DIRECTION ( 'NONE',  ( 0.000000000000000000, 0.000000000000000000, -1.000000000000000000 ) ) ;
#14622 = ADVANCED_FACE ( 'NONE', ( #9987 ), #12974, .T. ) ;
#14623 = ORIENTED_EDGE ( 'NONE', *, *, #4138, .F. ) ;
#14624 = EDGE_LOOP ( 'NONE', ( #10979, #8753, #3279, #10318, #1917, #13493 ) ) ;
#14625 = DIRECTION ( 'NONE',  ( 0.000000000000000000, 0.000000000000000000, 1.000000000000000000 ) ) ;
#14626 = DIRECTION ( 'NONE',  ( 0.000000000000000000, 0.000000000000000000, -1.000000000000000000 ) ) ;
#14627 = DIRECTION ( 'NONE',  ( -0.000000000000000000, -0.000000000000000000, 1.000000000000000000 ) ) ;
#14628 = ADVANCED_FACE ( 'NONE', ( #14867 ), #13074, .F. ) ;
#14629 = CARTESIAN_POINT ( 'NONE',  ( 11.17563879704982632, -2.222972771497745637, -20.91285899935257930 ) ) ;
#14630 = AXIS2_PLACEMENT_3D ( 'NONE', #7725, #14296, #20848 ) ;
#14631 = CARTESIAN_POINT ( 'NONE',  ( -6.330490856366290053, 9.474249098604506258, -3.294953500286802228 ) ) ;
#14632 = AXIS2_PLACEMENT_3D ( 'NONE', #18877, #2753, #9220 ) ;
#14633 = CARTESIAN_POINT ( 'NONE',  ( 19.99999999999999645, 0.000000000000000000, 0.000000000000000000 ) ) ;
#14634 = FACE_OUTER_BOUND ( 'NONE', #1463, .T. ) ;
#14635 = VERTEX_POINT ( 'NONE', #19736 ) ;
#14636 = DIRECTION ( 'NONE',  ( -1.000000000000000000, 0.000000000000000000, 0.000000000000000000 ) ) ;
#14637 = CARTESIAN_POINT ( 'NONE',  ( 3.580422610670020322, -18.00000000043041126, 6.520268750180314044 ) ) ;
#14638 = CARTESIAN_POINT ( 'NONE',  ( 19.99999999999999645, -31.98952867950285395, -56.39803944231618971 ) ) ;
#14639 = EDGE_LOOP ( 'NONE', ( #16094, #11892, #10349, #1725 ) ) ;
#14640 = PLANE ( 'NONE',  #4191 ) ;
#14641 = ORIENTED_EDGE ( 'NONE', *, *, #12066, .T. ) ;
#14642 = DIRECTION ( 'NONE',  ( 1.000000000000000000, 0.000000000000000000, 0.000000000000000000 ) ) ;
#14643 = CARTESIAN_POINT ( 'NONE',  ( 50.00000000000000000, 31.35083268962916137, -50.63110039191615641 ) ) ;
#14644 = EDGE_LOOP ( 'NONE', ( #6370, #16896, #4555, #12858 ) ) ;
#14645 = ORIENTED_EDGE ( 'NONE', *, *, #7119, .T. ) ;
#14646 = DIRECTION ( 'NONE',  ( 1.000000000000000000, 0.000000000000000000, 0.000000000000000000 ) ) ;
#14647 = CIRCLE ( 'NONE', #16679, 11.49999999999999645 ) ;
#14648 = AXIS2_PLACEMENT_3D ( 'NONE', #3859, #10336, #1440 ) ;
#14649 = EDGE_CURVE ( 'NONE', #6079, #12885, #18746, .T. ) ;
#14650 = TOROIDAL_SURFACE ( 'NONE', #18706, 11.17999999999999261, 0.3200000000000008393 ) ;
#14651 = AXIS2_PLACEMENT_3D ( 'NONE', #12704, #11105, #17578 ) ;
#14652 = DIRECTION ( 'NONE',  ( 0.000000000000000000, 0.000000000000000000, 1.000000000000000000 ) ) ;
#14653 = ADVANCED_FACE ( 'NONE', ( #14663 ), #16049, .T. ) ;
#14654 = EDGE_CURVE ( 'NONE', #7362, #6859, #9601, .T. ) ;
#14655 = DIRECTION ( 'NONE',  ( -0.000000000000000000, -0.000000000000000000, -1.000000000000000000 ) ) ;
#14656 = ORIENTED_EDGE ( 'NONE', *, *, #12846, .F. ) ;
#14657 = CARTESIAN_POINT ( 'NONE',  ( 6.358192987158590270, -4.248408730893245000, 10.68239375018031190 ) ) ;
#14658 = EDGE_CURVE ( 'NONE', #17751, #1745, #17947, .T. ) ;
#14659 = PLANE ( 'NONE',  #3391 ) ;
#14660 = EDGE_CURVE ( 'NONE', #20532, #12434, #1649, .T. ) ;
#14661 = AXIS2_PLACEMENT_3D ( 'NONE', #16063, #4401, #1556 ) ;
#14662 = DIRECTION ( 'NONE',  ( 0.000000000000000000, 0.000000000000000000, 1.000000000000000000 ) ) ;
#14663 = FACE_OUTER_BOUND ( 'NONE', #3937, .T. ) ;
#14664 = AXIS2_PLACEMENT_3D ( 'NONE', #9386, #15847, #20706 ) ;
#14665 = ORIENTED_EDGE ( 'NONE', *, *, #16366, .F. ) ;
#14666 = CARTESIAN_POINT ( 'NONE',  ( 15.25966316918061416, -10.19618095414378622, -22.93285624981968951 ) ) ;
#14667 = VERTEX_POINT ( 'NONE', #19428 ) ;
#14668 = CARTESIAN_POINT ( 'NONE',  ( 6.888301784570728614, 16.62983158437510056, 19.63676250018031766 ) ) ;
#14669 = DIRECTION ( 'NONE',  ( 0.000000000000000000, 0.000000000000000000, -1.000000000000000000 ) ) ;
#14670 = VERTEX_POINT ( 'NONE', #14567 ) ;
#14671 = DIRECTION ( 'NONE',  ( 0.000000000000000000, 1.040834085586084454E-15, -1.000000000000000000 ) ) ;
#14672 = ORIENTED_EDGE ( 'NONE', *, *, #11286, .T. ) ;
#14673 = DIRECTION ( 'NONE',  ( -1.000000000000000000, 0.000000000000000000, 0.000000000000000000 ) ) ;
#14674 =( BOUNDED_SURFACE ( )  B_SPLINE_SURFACE ( 3, 2, ( 
 ( #4907, #2032, #9982, #17852, #3511, #451, #19425, #11783, #11375, #8093, #16446, #16548, #8391, #3617, #6483, #241, #13174, #19622, #3712, #16345, #5101, #13070, #3321, #19529, #11572, #9781, #16151, #1933, #1836, #14657, #6789, #10091, #14864, #338, #6901, #135, #6587, #5314, #13275, #16247, #1645, #19731, #14564, #9878, #5214, #31, #12970, #11677, #18145, #8483, #5013, #3410, #11474, #8287, #13386, #10505, #13805, #15269, #2140, #19930, #7207, #757, #18350, #12103, #10302, #13580, #10408, #15072, #5723, #5407, #18665, #2448, #20137, #4135, #3816, #980, #11879, #13901, #15490, #10622, #9028, #13693, #651, #7423, #5622, #4028, #8912, #16965, #555, #20251, #16870, #11992, #15383, #16760, #17081, #866, #2242, #18569, #20350, #13487, #5835, #8704, #8599, #7318, #2564, #12196, #12312, #7005, #18782, #10189, #16653, #15173, #2346, #7100, #20029, #5511, #18457, #8795, #3924, #4250, #7749, #4460, #17293, #15904, #12744, #14222, #19100, #9544, #2769, #9234, #14437, #20667, #14015, #6365, #9445, #17196, #18986, #2984, #20883, #10731, #1401, #9339, #11034, #9130, #12524, #20466, #15697, #1513, #4572, #7851, #15802, #2670, #5944, #1306, #6150, #12419, #12638, #4360, #7641, #10928, #15587 ),
 ( #19198, #18894, #16014, #10825, #7964, #12845, #4678, #3079, #17511, #1194, #1084, #14332, #20779, #6261, #11139, #17609, #17405, #7529, #14121, #20574, #6050, #2874, #19603, #213, #13249, #19702, #19394, #16529, #9956, #14737, #317, #6769, #5181, #8462, #6670, #18124, #8069, #10069, #11456, #19500, #4989, #4884, #18016, #11653, #6565, #3385, #3591, #2013, #14943, #11352, #4772, #5078, #19288, #16124, #421, #6872, #11239, #14538, #8371, #17717, #3190, #9659, #1616, #17824, #13153, #4, #6458, #12944, #17924, #3296, #9759, #16224, #1708, #11543, #8158, #14631, #110, #13047, #3482, #9850, #16318, #1810, #8264, #16420, #1906, #14842, #20118, #20230, #2114, #633, #7186, #16942, #8887, #19910, #8777, #8675, #17057, #10381, #6977, #5597, #15247, #2543, #13359, #7297, #18548, #13466, #530, #12078, #961, #5388, #2324, #8572, #845, #4003, #19807, #10486, #11762, #9004, #15470, #3693, #5289, #731, #15048, #5702, #11857, #18326, #15151, #3793, #18228, #11967, #10165, #18437, #16626, #3901, #5489, #10274, #7079, #16737, #2218, #13559, #20005, #16846, #2424, #13669, #10595, #15361, #13779, #18643, #12175, #4111, #9520, #20446, #15883, #17170, #14305, #14204, #6236, #4655, #2745, #9427, #10707 ),
 ( #12606, #20324, #1174, #6127, #17590, #7403, #19073, #12504, #20647, #12286, #15671, #11119, #7731, #11007, #18966, #5810, #2653, #4438, #10904, #15565, #9317, #7503, #10808, #7618, #18761, #2961, #9110, #1379, #4548, #17379, #7826, #1058, #19173, #13990, #3057, #12720, #20749, #15986, #2850, #18868, #13880, #15780, #1282, #17486, #4229, #5925, #14098, #12396, #4342, #17272, #9211, #20550, #6032, #3362, #16396, #1881, #1591, #19673, #13130, #17901, #3459, #9929, #8344, #11627, #9825, #293, #11216, #13224, #14608, #1687, #8135, #8044, #186, #14820, #9735, #6541, #6743, #5152, #18100, #14517, #12826, #11517, #83, #3267, #8238, #17691, #3564, #16293, #3164, #1782, #10044, #4748, #1489, #9636, #14413, #14715, #7938, #6646, #20857, #19269, #13024, #19476, #4961, #6341, #11431, #19579, #19369, #16099, #4859, #5054, #12016, #6434, #17991, #12918, #11329, #17797, #16200, #5464, #10353, #821, #8542, #15024, #5679, #19981, #5264, #18619, #705, #8440, #10247, #15223, #12151, #16510, #7160, #614, #2304, #392, #3766, #11737, #6953, #18206, #7267, #8648, #16711, #2192, #16597, #13642, #3983, #15127, #7057, #13747, #20202, #2400, #2087, #6844, #5568, #13537, #18300, #8756, #3670, #8860, #16822 ),
 ( #11937, #507, #18411, #4082, #13441, #1992, #10145, #3875, #20090, #14916, #13334, #19892, #12049, #19784, #5366, #11835, #18520, #10462, #16919, #15332, #15754, #14072, #7708, #6099, #1030, #17350, #7376, #10680, #15537, #1254, #4315, #2625, #2824, #15645, #18838, #4410, #10877, #7594, #20297, #7478, #20623, #9086, #13961, #20415, #17030, #20523, #10565, #13852, #4520, #14182, #15438, #5780, #9293, #12577, #10985, #2517, #8974, #5900, #6005, #18730, #4203, #930, #12477, #12372, #12256, #17140, #10783, #17245, #2715, #9183, #18941, #19045, #1143, #18692, #15091, #889, #579, #8818, #18266, #5335, #15293, #15405, #3732, #16780, #2367, #12122, #4050, #7029, #3946, #3840, #12222, #5534, #2162, #781, #10431, #4163, #8507, #2476, #13713, #8617, #16675, #20269, #19949, #11898, #2268, #14988, #7229, #473, #11802, #10647, #16989, #6922, #10211, #18590, #8936, #17103, #13406, #19857, #13506, #16891, #5428, #18372, #10321, #670, #8728, #15193, #7343, #7123, #20159, #13826, #10530, #13603, #20052, #5646, #12013, #18479, #5747, #9150, #2897, #12336, #20377, #9363, #9464, #18803, #10845, #17429, #6173, #19120, #15607, #19007, #18912, #6281, #20593, #17215, #15826, #4484, #12769, #2585, #17535, #7769, #2689 ) ),
 .UNSPECIFIED., .F., .F., .T. ) 
 B_SPLINE_SURFACE_WITH_KNOTS ( ( 4, 4 ),
 ( 3, 2, 2, 2, 2, 2, 2, 2, 2, 2, 2, 2, 2, 2, 2, 2, 2, 2, 2, 2, 2, 2, 2, 2, 2, 2, 2, 2, 2, 2, 2, 2, 2, 2, 2, 2, 2, 2, 2, 2, 2, 2, 2, 2, 2, 2, 2, 2, 2, 2, 2, 2, 2, 2, 2, 2, 2, 2, 2, 2, 2, 2, 2, 2, 2, 2, 2, 2, 2, 2, 2, 2, 2, 2, 2, 2, 2, 2, 2, 2, 3 ),
 ( 0.000000000000000000, 1.000000000000000000 ),
 ( 0.000000000000000000, 0.01250000000000000069, 0.02500000000000000139, 0.03749999999999999861, 0.05000000000000000278, 0.06250000000000000000, 0.07499999999999999722, 0.08749999999999999445, 0.1000000000000000056, 0.1125000000000000028, 0.1250000000000000000, 0.1375000000000000111, 0.1499999999999999944, 0.1625000000000000056, 0.1749999999999999889, 0.1875000000000000000, 0.2000000000000000111, 0.2124999999999999944, 0.2250000000000000056, 0.2374999999999999889, 0.2500000000000000000, 0.2625000000000000111, 0.2750000000000000222, 0.2874999999999999778, 0.2999999999999999889, 0.3125000000000000000, 0.3250000000000000111, 0.3375000000000000222, 0.3499999999999999778, 0.3624999999999999889, 0.3750000000000000000, 0.3875000000000000111, 0.4000000000000000222, 0.4124999999999999778, 0.4249999999999999889, 0.4375000000000000000, 0.4500000000000000111, 0.4625000000000000222, 0.4749999999999999778, 0.4874999999999999889, 0.5000000000000000000, 0.5124999999999999556, 0.5250000000000000222, 0.5374999999999999778, 0.5500000000000000444, 0.5625000000000000000, 0.5749999999999999556, 0.5875000000000000222, 0.5999999999999999778, 0.6125000000000000444, 0.6250000000000000000, 0.6374999999999999556, 0.6500000000000000222, 0.6624999999999999778, 0.6750000000000000444, 0.6875000000000000000, 0.6999999999999999556, 0.7125000000000000222, 0.7249999999999999778, 0.7375000000000000444, 0.7500000000000000000, 0.7624999999999999556, 0.7750000000000000222, 0.7874999999999999778, 0.8000000000000000444, 0.8125000000000000000, 0.8249999999999999556, 0.8375000000000000222, 0.8499999999999999778, 0.8625000000000000444, 0.8750000000000000000, 0.8874999999999999556, 0.9000000000000000222, 0.9124999999999999778, 0.9250000000000000444, 0.9375000000000000000, 0.9499999999999999556, 0.9625000000000000222, 0.9749999999999999778, 0.9875000000000000444, 1.000000000000000000 ),
 .UNSPECIFIED. ) 
 GEOMETRIC_REPRESENTATION_ITEM ( )  RATIONAL_B_SPLINE_SURFACE ( (
 ( 1.000000000000000000, 0.9807852804032304306, 1.000000000000000000, 0.9807852804032304306, 1.000000000000000000, 0.9807852804032304306, 1.000000000000000000, 0.9807852804032304306, 1.000000000000000000, 0.9807852804032304306, 1.000000000000000000, 0.9807852804032304306, 1.000000000000000000, 0.9807852804032304306, 1.000000000000000000, 0.9807852804032304306, 1.000000000000000000, 0.9807852804032304306, 1.000000000000000000, 0.9807852804032304306, 1.000000000000000000, 0.9807852804032304306, 1.000000000000000000, 0.9807852804032304306, 1.000000000000000000, 0.9807852804032304306, 1.000000000000000000, 0.9807852804032304306, 1.000000000000000000, 0.9807852804032304306, 1.000000000000000000, 0.9807852804032304306, 1.000000000000000000, 0.9807852804032304306, 1.000000000000000000, 0.9807852804032304306, 1.000000000000000000, 0.9807852804032304306, 1.000000000000000000, 0.9807852804032304306, 1.000000000000000000, 0.9807852804032304306, 1.000000000000000000, 0.9807852804032304306, 1.000000000000000000, 0.9807852804032304306, 1.000000000000000000, 0.9807852804032304306, 1.000000000000000000, 0.9807852804032304306, 1.000000000000000000, 0.9807852804032304306, 1.000000000000000000, 0.9807852804032304306, 1.000000000000000000, 0.9807852804032304306, 1.000000000000000000, 0.9807852804032304306, 1.000000000000000000, 0.9807852804032304306, 1.000000000000000000, 0.9807852804032304306, 1.000000000000000000, 0.9807852804032304306, 1.000000000000000000, 0.9807852804032304306, 1.000000000000000000, 0.9807852804032304306, 1.000000000000000000, 0.9807852804032304306, 1.000000000000000000, 0.9807852804032304306, 1.000000000000000000, 0.9807852804032304306, 1.000000000000000000, 0.9807852804032304306, 1.000000000000000000, 0.9807852804032304306, 1.000000000000000000, 0.9807852804032304306, 1.000000000000000000, 0.9807852804032304306, 1.000000000000000000, 0.9807852804032304306, 1.000000000000000000, 0.9807852804032304306, 1.000000000000000000, 0.9807852804032304306, 1.000000000000000000, 0.9807852804032304306, 1.000000000000000000, 0.9807852804032304306, 1.000000000000000000, 0.9807852804032304306, 1.000000000000000000, 0.9807852804032304306, 1.000000000000000000, 0.9807852804032304306, 1.000000000000000000, 0.9807852804032304306, 1.000000000000000000, 0.9807852804032304306, 1.000000000000000000, 0.9807852804032304306, 1.000000000000000000, 0.9807852804032304306, 1.000000000000000000, 0.9807852804032304306, 1.000000000000000000, 0.9807852804032304306, 1.000000000000000000, 0.9807852804032304306, 1.000000000000000000, 0.9807852804032304306, 1.000000000000000000, 0.9807852804032304306, 1.000000000000000000, 0.9807852804032304306, 1.000000000000000000, 0.9807852804032304306, 1.000000000000000000, 0.9807852804032304306, 1.000000000000000000, 0.9807852804032304306, 1.000000000000000000, 0.9807852804032304306, 1.000000000000000000, 0.9807852804032304306, 1.000000000000000000, 0.9807852804032304306, 1.000000000000000000, 0.9807852804032304306, 1.000000000000000000, 0.9807852804032304306, 1.000000000000000000, 0.9807852804032304306, 1.000000000000000000, 0.9807852804032304306, 1.000000000000000000, 0.9807852804032304306, 1.000000000000000000, 0.9807852804032304306, 1.000000000000000000, 0.9807852804032304306, 1.000000000000000000, 0.9807852804032304306, 1.000000000000000000, 0.9807852804032304306, 1.000000000000000000, 0.9807852804032304306, 1.000000000000000000, 0.9807852804032304306, 1.000000000000000000, 0.9807852804032304306, 1.000000000000000000, 0.9807852804032304306, 1.000000000000000000, 0.9807852804032304306, 1.000000000000000000, 0.9807852804032304306, 1.000000000000000000),
 ( 0.9659702800374152520, 0.9474094319676833464, 0.9659702800374152520, 0.9474094319676833464, 0.9659702800374152520, 0.9474094319676833464, 0.9659702800374152520, 0.9474094319676833464, 0.9659702800374152520, 0.9474094319676833464, 0.9659702800374152520, 0.9474094319676833464, 0.9659702800374152520, 0.9474094319676833464, 0.9659702800374152520, 0.9474094319676833464, 0.9659702800374152520, 0.9474094319676833464, 0.9659702800374152520, 0.9474094319676833464, 0.9659702800374152520, 0.9474094319676833464, 0.9659702800374152520, 0.9474094319676833464, 0.9659702800374152520, 0.9474094319676833464, 0.9659702800374152520, 0.9474094319676833464, 0.9659702800374152520, 0.9474094319676833464, 0.9659702800374152520, 0.9474094319676833464, 0.9659702800374152520, 0.9474094319676833464, 0.9659702800374152520, 0.9474094319676833464, 0.9659702800374152520, 0.9474094319676833464, 0.9659702800374152520, 0.9474094319676833464, 0.9659702800374152520, 0.9474094319676833464, 0.9659702800374152520, 0.9474094319676833464, 0.9659702800374152520, 0.9474094319676833464, 0.9659702800374152520, 0.9474094319676833464, 0.9659702800374152520, 0.9474094319676833464, 0.9659702800374152520, 0.9474094319676833464, 0.9659702800374152520, 0.9474094319676833464, 0.9659702800374152520, 0.9474094319676833464, 0.9659702800374152520, 0.9474094319676833464, 0.9659702800374152520, 0.9474094319676833464, 0.9659702800374152520, 0.9474094319676833464, 0.9659702800374152520, 0.9474094319676833464, 0.9659702800374152520, 0.9474094319676833464, 0.9659702800374152520, 0.9474094319676833464, 0.9659702800374152520, 0.9474094319676833464, 0.9659702800374152520, 0.9474094319676833464, 0.9659702800374152520, 0.9474094319676833464, 0.9659702800374152520, 0.9474094319676833464, 0.9659702800374152520, 0.9474094319676833464, 0.9659702800374152520, 0.9474094319676833464, 0.9659702800374152520, 0.9474094319676833464, 0.9659702800374152520, 0.9474094319676833464, 0.9659702800374152520, 0.9474094319676833464, 0.9659702800374152520, 0.9474094319676833464, 0.9659702800374152520, 0.9474094319676833464, 0.9659702800374152520, 0.9474094319676833464, 0.9659702800374152520, 0.9474094319676833464, 0.9659702800374152520, 0.9474094319676833464, 0.9659702800374152520, 0.9474094319676833464, 0.9659702800374152520, 0.9474094319676833464, 0.9659702800374152520, 0.9474094319676833464, 0.9659702800374152520, 0.9474094319676833464, 0.9659702800374152520, 0.9474094319676833464, 0.9659702800374152520, 0.9474094319676833464, 0.9659702800374152520, 0.9474094319676833464, 0.9659702800374152520, 0.9474094319676833464, 0.9659702800374152520, 0.9474094319676833464, 0.9659702800374152520, 0.9474094319676833464, 0.9659702800374152520, 0.9474094319676833464, 0.9659702800374152520, 0.9474094319676833464, 0.9659702800374152520, 0.9474094319676833464, 0.9659702800374152520, 0.9474094319676833464, 0.9659702800374152520, 0.9474094319676833464, 0.9659702800374152520, 0.9474094319676833464, 0.9659702800374152520, 0.9474094319676833464, 0.9659702800374152520, 0.9474094319676833464, 0.9659702800374152520, 0.9474094319676833464, 0.9659702800374152520, 0.9474094319676833464, 0.9659702800374152520, 0.9474094319676833464, 0.9659702800374152520, 0.9474094319676833464, 0.9659702800374152520, 0.9474094319676833464, 0.9659702800374152520, 0.9474094319676833464, 0.9659702800374152520, 0.9474094319676833464, 0.9659702800374152520, 0.9474094319676833464, 0.9659702800374152520, 0.9474094319676833464, 0.9659702800374152520, 0.9474094319676833464, 0.9659702800374152520, 0.9474094319676833464, 0.9659702800374152520, 0.9474094319676833464, 0.9659702800374152520, 0.9474094319676833464, 0.9659702800374152520, 0.9474094319676833464, 0.9659702800374152520),
 ( 0.9659702800374152520, 0.9474094319676833464, 0.9659702800374152520, 0.9474094319676833464, 0.9659702800374152520, 0.9474094319676833464, 0.9659702800374152520, 0.9474094319676833464, 0.9659702800374152520, 0.9474094319676833464, 0.9659702800374152520, 0.9474094319676833464, 0.9659702800374152520, 0.9474094319676833464, 0.9659702800374152520, 0.9474094319676833464, 0.9659702800374152520, 0.9474094319676833464, 0.9659702800374152520, 0.9474094319676833464, 0.9659702800374152520, 0.9474094319676833464, 0.9659702800374152520, 0.9474094319676833464, 0.9659702800374152520, 0.9474094319676833464, 0.9659702800374152520, 0.9474094319676833464, 0.9659702800374152520, 0.9474094319676833464, 0.9659702800374152520, 0.9474094319676833464, 0.9659702800374152520, 0.9474094319676833464, 0.9659702800374152520, 0.9474094319676833464, 0.9659702800374152520, 0.9474094319676833464, 0.9659702800374152520, 0.9474094319676833464, 0.9659702800374152520, 0.9474094319676833464, 0.9659702800374152520, 0.9474094319676833464, 0.9659702800374152520, 0.9474094319676833464, 0.9659702800374152520, 0.9474094319676833464, 0.9659702800374152520, 0.9474094319676833464, 0.9659702800374152520, 0.9474094319676833464, 0.9659702800374152520, 0.9474094319676833464, 0.9659702800374152520, 0.9474094319676833464, 0.9659702800374152520, 0.9474094319676833464, 0.9659702800374152520, 0.9474094319676833464, 0.9659702800374152520, 0.9474094319676833464, 0.9659702800374152520, 0.9474094319676833464, 0.9659702800374152520, 0.9474094319676833464, 0.9659702800374152520, 0.9474094319676833464, 0.9659702800374152520, 0.9474094319676833464, 0.9659702800374152520, 0.9474094319676833464, 0.9659702800374152520, 0.9474094319676833464, 0.9659702800374152520, 0.9474094319676833464, 0.9659702800374152520, 0.9474094319676833464, 0.9659702800374152520, 0.9474094319676833464, 0.9659702800374152520, 0.9474094319676833464, 0.9659702800374152520, 0.9474094319676833464, 0.9659702800374152520, 0.9474094319676833464, 0.9659702800374152520, 0.9474094319676833464, 0.9659702800374152520, 0.9474094319676833464, 0.9659702800374152520, 0.9474094319676833464, 0.9659702800374152520, 0.9474094319676833464, 0.9659702800374152520, 0.9474094319676833464, 0.9659702800374152520, 0.9474094319676833464, 0.9659702800374152520, 0.9474094319676833464, 0.9659702800374152520, 0.9474094319676833464, 0.9659702800374152520, 0.9474094319676833464, 0.9659702800374152520, 0.9474094319676833464, 0.9659702800374152520, 0.9474094319676833464, 0.9659702800374152520, 0.9474094319676833464, 0.9659702800374152520, 0.9474094319676833464, 0.9659702800374152520, 0.9474094319676833464, 0.9659702800374152520, 0.9474094319676833464, 0.9659702800374152520, 0.9474094319676833464, 0.9659702800374152520, 0.9474094319676833464, 0.9659702800374152520, 0.9474094319676833464, 0.9659702800374152520, 0.9474094319676833464, 0.9659702800374152520, 0.9474094319676833464, 0.9659702800374152520, 0.9474094319676833464, 0.9659702800374152520, 0.9474094319676833464, 0.9659702800374152520, 0.9474094319676833464, 0.9659702800374152520, 0.9474094319676833464, 0.9659702800374152520, 0.9474094319676833464, 0.9659702800374152520, 0.9474094319676833464, 0.9659702800374152520, 0.9474094319676833464, 0.9659702800374152520, 0.9474094319676833464, 0.9659702800374152520, 0.9474094319676833464, 0.9659702800374152520, 0.9474094319676833464, 0.9659702800374152520, 0.9474094319676833464, 0.9659702800374152520, 0.9474094319676833464, 0.9659702800374152520, 0.9474094319676833464, 0.9659702800374152520, 0.9474094319676833464, 0.9659702800374152520, 0.9474094319676833464, 0.9659702800374152520, 0.9474094319676833464, 0.9659702800374152520, 0.9474094319676833464, 0.9659702800374152520),
 ( 1.000000000000000000, 0.9807852804032304306, 1.000000000000000000, 0.9807852804032304306, 1.000000000000000000, 0.9807852804032304306, 1.000000000000000000, 0.9807852804032304306, 1.000000000000000000, 0.9807852804032304306, 1.000000000000000000, 0.9807852804032304306, 1.000000000000000000, 0.9807852804032304306, 1.000000000000000000, 0.9807852804032304306, 1.000000000000000000, 0.9807852804032304306, 1.000000000000000000, 0.9807852804032304306, 1.000000000000000000, 0.9807852804032304306, 1.000000000000000000, 0.9807852804032304306, 1.000000000000000000, 0.9807852804032304306, 1.000000000000000000, 0.9807852804032304306, 1.000000000000000000, 0.9807852804032304306, 1.000000000000000000, 0.9807852804032304306, 1.000000000000000000, 0.9807852804032304306, 1.000000000000000000, 0.9807852804032304306, 1.000000000000000000, 0.9807852804032304306, 1.000000000000000000, 0.9807852804032304306, 1.000000000000000000, 0.9807852804032304306, 1.000000000000000000, 0.9807852804032304306, 1.000000000000000000, 0.9807852804032304306, 1.000000000000000000, 0.9807852804032304306, 1.000000000000000000, 0.9807852804032304306, 1.000000000000000000, 0.9807852804032304306, 1.000000000000000000, 0.9807852804032304306, 1.000000000000000000, 0.9807852804032304306, 1.000000000000000000, 0.9807852804032304306, 1.000000000000000000, 0.9807852804032304306, 1.000000000000000000, 0.9807852804032304306, 1.000000000000000000, 0.9807852804032304306, 1.000000000000000000, 0.9807852804032304306, 1.000000000000000000, 0.9807852804032304306, 1.000000000000000000, 0.9807852804032304306, 1.000000000000000000, 0.9807852804032304306, 1.000000000000000000, 0.9807852804032304306, 1.000000000000000000, 0.9807852804032304306, 1.000000000000000000, 0.9807852804032304306, 1.000000000000000000, 0.9807852804032304306, 1.000000000000000000, 0.9807852804032304306, 1.000000000000000000, 0.9807852804032304306, 1.000000000000000000, 0.9807852804032304306, 1.000000000000000000, 0.9807852804032304306, 1.000000000000000000, 0.9807852804032304306, 1.000000000000000000, 0.9807852804032304306, 1.000000000000000000, 0.9807852804032304306, 1.000000000000000000, 0.9807852804032304306, 1.000000000000000000, 0.9807852804032304306, 1.000000000000000000, 0.9807852804032304306, 1.000000000000000000, 0.9807852804032304306, 1.000000000000000000, 0.9807852804032304306, 1.000000000000000000, 0.9807852804032304306, 1.000000000000000000, 0.9807852804032304306, 1.000000000000000000, 0.9807852804032304306, 1.000000000000000000, 0.9807852804032304306, 1.000000000000000000, 0.9807852804032304306, 1.000000000000000000, 0.9807852804032304306, 1.000000000000000000, 0.9807852804032304306, 1.000000000000000000, 0.9807852804032304306, 1.000000000000000000, 0.9807852804032304306, 1.000000000000000000, 0.9807852804032304306, 1.000000000000000000, 0.9807852804032304306, 1.000000000000000000, 0.9807852804032304306, 1.000000000000000000, 0.9807852804032304306, 1.000000000000000000, 0.9807852804032304306, 1.000000000000000000, 0.9807852804032304306, 1.000000000000000000, 0.9807852804032304306, 1.000000000000000000, 0.9807852804032304306, 1.000000000000000000, 0.9807852804032304306, 1.000000000000000000, 0.9807852804032304306, 1.000000000000000000, 0.9807852804032304306, 1.000000000000000000, 0.9807852804032304306, 1.000000000000000000, 0.9807852804032304306, 1.000000000000000000, 0.9807852804032304306, 1.000000000000000000, 0.9807852804032304306, 1.000000000000000000, 0.9807852804032304306, 1.000000000000000000, 0.9807852804032304306, 1.000000000000000000, 0.9807852804032304306, 1.000000000000000000, 0.9807852804032304306, 1.000000000000000000) ) ) 
 REPRESENTATION_ITEM ( '' )  SURFACE ( )  );
#14675 = CIRCLE ( 'NONE', #10948, 72.00000000007199219 ) ;
#14676 = EDGE_LOOP ( 'NONE', ( #14139, #6795, #9924, #17551 ) ) ;
#14677 = EDGE_CURVE ( 'NONE', #16808, #15390, #20431, .T. ) ;
#14678 = DIRECTION ( 'NONE',  ( 0.000000000000000000, -6.982962677686266711E-15, 1.000000000000000000 ) ) ;
#14679 = AXIS2_PLACEMENT_3D ( 'NONE', #3430, #13195, #155 ) ;
#14680 = AXIS2_PLACEMENT_3D ( 'NONE', #8784, #18558, #18337 ) ;
#14681 = EDGE_CURVE ( 'NONE', #15235, #5163, #8191, .T. ) ;
#14682 = ADVANCED_FACE ( 'NONE', ( #2247 ), #2350, .T. ) ;
#14683 = CARTESIAN_POINT ( 'NONE',  ( 40.00000000000000711, -122.3205080756887781, -90.00000000000001421 ) ) ;
#14684 = CARTESIAN_POINT ( 'NONE',  ( 13.67243654778935991, 5.663308646854338768, -13.12377058115845863 ) ) ;
#14685 = ORIENTED_EDGE ( 'NONE', *, *, #16466, .F. ) ;
#14687 = EDGE_CURVE ( 'NONE', #19384, #10000, #1496, .T. ) ;
#14686 = CARTESIAN_POINT ( 'NONE',  ( -3.344563996438217224, -2.687817229851499068, -5.441324518471498450 ) ) ;
#14688 = FACE_OUTER_BOUND ( 'NONE', #3049, .T. ) ;
#14689 = VERTEX_POINT ( 'NONE', #870 ) ;
#14690 = AXIS2_PLACEMENT_3D ( 'NONE', #4602, #15934, #1431 ) ;
#14691 = CARTESIAN_POINT ( 'NONE',  ( 3.600000000000066702, 10.82531754730546147, 126.0000000000000000 ) ) ;
#14692 = CARTESIAN_POINT ( 'NONE',  ( -10.19618095047498052, 15.25966317163203101, 20.06870625018031262 ) ) ;
#14693 = LINE ( 'NONE', #164, #2237 ) ;
#14694 = LINE ( 'NONE', #2065, #20167 ) ;
#14695 = AXIS2_PLACEMENT_3D ( 'NONE', #12547, #14465, #20909 ) ;
#14696 = ORIENTED_EDGE ( 'NONE', *, *, #3673, .T. ) ;
#14697 = AXIS2_PLACEMENT_3D ( 'NONE', #41, #13701, #2458 ) ;
#14698 = CARTESIAN_POINT ( 'NONE',  ( -2.678494666091065124, -3.072372537026387018, -0.03421028094655000767 ) ) ;
#14699 = ORIENTED_EDGE ( 'NONE', *, *, #5420, .T. ) ;
#14700 = SURFACE_STYLE_USAGE ( .BOTH. , #5353 ) ;
#14701 = EDGE_CURVE ( 'NONE', #17868, #14994, #11969, .T. ) ;
#14702 = CARTESIAN_POINT ( 'NONE',  ( 1.040949779275250179E-14, -85.00000000000000000, 5.000000000000000000 ) ) ;
#14703 = CARTESIAN_POINT ( 'NONE',  ( 29.99999999999966249, -160.0000000000000000, 53.99496054166689163 ) ) ;
#14704 = VECTOR ( 'NONE', #7770, 1000.000000000000000 ) ;
#14705 = VERTEX_POINT ( 'NONE', #16552 ) ;
#14706 = CARTESIAN_POINT ( 'NONE',  ( 19.99999999999999645, 1.971042061629218356, -64.80882494896104618 ) ) ;
#14707 = CARTESIAN_POINT ( 'NONE',  ( 29.99999999999965183, -159.9999999999999716, 53.99496054166689873 ) ) ;
#14708 = DIRECTION ( 'NONE',  ( -9.719167153370763981E-31, -1.472034489194787016E-30, 1.000000000000000000 ) ) ;
#14709 = VECTOR ( 'NONE', #137, 1000.000000000000000 ) ;
#14710 = CARTESIAN_POINT ( 'NONE',  ( -2.163827323447878648E-09, -18.00000000000000355, -12.03519999981969590 ) ) ;
#14711 = ORIENTED_EDGE ( 'NONE', *, *, #12340, .F. ) ;
#14712 = AXIS2_PLACEMENT_3D ( 'NONE', #15368, #13567, #11975 ) ;
#14713 = CARTESIAN_POINT ( 'NONE',  ( -7.500000000000000888, -3.289131931895657122E-15, 5.086300000002307087 ) ) ;
#14714 = FACE_BOUND ( 'NONE', #878, .T. ) ;
#14715 = CARTESIAN_POINT ( 'NONE',  ( 14.79893867722909917, -2.943691928843437111, -8.433260668480928146 ) ) ;
#14716 = EDGE_CURVE ( 'NONE', #17222, #3247, #13585, .T. ) ;
#14717 = DIRECTION ( 'NONE',  ( 0.000000000000000000, 0.000000000000000000, -1.000000000000000000 ) ) ;
#14718 = ORIENTED_EDGE ( 'NONE', *, *, #10921, .T. ) ;
#14719 = CARTESIAN_POINT ( 'NONE',  ( 19.99999999999999645, -15.58726123847806200, -62.93731870009420959 ) ) ;
#14720 = DIRECTION ( 'NONE',  ( -0.000000000000000000, -0.000000000000000000, 1.000000000000000000 ) ) ;
#14721 = DIRECTION ( 'NONE',  ( 0.000000000000000000, 0.000000000000000000, 1.000000000000000000 ) ) ;
#14722 = VERTEX_POINT ( 'NONE', #11883 ) ;
#14723 = CARTESIAN_POINT ( 'NONE',  ( -11.50000000000000000, 1.408343819019456176E-15, 81.99999999999998579 ) ) ;
#14724 = ORIENTED_EDGE ( 'NONE', *, *, #8792, .T. ) ;
#14725 = MECHANICAL_DESIGN_GEOMETRIC_PRESENTATION_REPRESENTATION (  '', ( #162 ), #8640 ) ;
#14726 = CARTESIAN_POINT ( 'NONE',  ( 2.500000000000000000, 0.000000000000000000, 0.000000000000000000 ) ) ;
#14727 = CARTESIAN_POINT ( 'NONE',  ( 0.000000000000000000, 56.63599015375715595, -31.56633360682406675 ) ) ;
#14728 = VERTEX_POINT ( 'NONE', #15273 ) ;
#14729 = ORIENTED_EDGE ( 'NONE', *, *, #3350, .T. ) ;
#14730 = CARTESIAN_POINT ( 'NONE',  ( 19.99999999999999645, 0.000000000000000000, 0.000000000000000000 ) ) ;
#14731 = CARTESIAN_POINT ( 'NONE',  ( 2.500000000000000000, 0.000000000000000000, 0.000000000000000000 ) ) ;
#14732 = CARTESIAN_POINT ( 'NONE',  ( 10.19618095414378978, 15.25966316918061771, -15.86410624981969697 ) ) ;
#14733 = CARTESIAN_POINT ( 'NONE',  ( 0.2500000000000002220, 0.000000000000000000, 0.000000000000000000 ) ) ;
#14734 = CARTESIAN_POINT ( 'NONE',  ( 30.00000000000000355, -139.6410161513775563, -90.00000000000001421 ) ) ;
#14735 = CARTESIAN_POINT ( 'NONE',  ( 7.500000000179346316, 1.491842754445843244, 15.76916875018031305 ) ) ;
#14736 = CIRCLE ( 'NONE', #20827, 2.649999999999988365 ) ;
#14737 = CARTESIAN_POINT ( 'NONE',  ( 9.474249097082495297, -6.330490858644137298, 10.25348399971320035 ) ) ;
#14738 = EDGE_CURVE ( 'NONE', #19110, #12652, #761, .T. ) ;
#14739 = CARTESIAN_POINT ( 'NONE',  ( -6.999999999999993783, -11.17999999999998906, 1.388749470233097779E-15 ) ) ;
#14740 = DIRECTION ( 'NONE',  ( 0.000000000000000000, -0.6310879443260593025, 0.7757112907044145800 ) ) ;
#14741 = ORIENTED_EDGE ( 'NONE', *, *, #10414, .F. ) ;
#14742 = DIRECTION ( 'NONE',  ( 0.000000000000000000, 0.8878852184023764416, -0.4600650377311500394 ) ) ;
#14743 = CARTESIAN_POINT ( 'NONE',  ( -17.99999999956958519, 3.580422614997674113, 9.465581250180312267 ) ) ;
#14744 = DIRECTION ( 'NONE',  ( -0.000000000000000000, -0.000000000000000000, 1.000000000000000000 ) ) ;
#14745 = ORIENTED_EDGE ( 'NONE', *, *, #13859, .F. ) ;
#14746 = CARTESIAN_POINT ( 'NONE',  ( -12.50000000000000533, 0.000000000000000000, -40.00000000000000000 ) ) ;
#14747 = VERTEX_POINT ( 'NONE', #8709 ) ;
#14748 = DIRECTION ( 'NONE',  ( 0.000000000000000000, 0.000000000000000000, 1.000000000000000000 ) ) ;
#14749 = CARTESIAN_POINT ( 'NONE',  ( 35.80519692130376797, -23.36569907514590838, 75.18387685020788069 ) ) ;
#14750 = AXIS2_PLACEMENT_3D ( 'NONE', #12541, #20903, #4478 ) ;
#14751 = ORIENTED_EDGE ( 'NONE', *, *, #16207, .T. ) ;
#14752 = ORIENTED_EDGE ( 'NONE', *, *, #10122, .T. ) ;
#14753 = CYLINDRICAL_SURFACE ( 'NONE', #18839, 72.00000000007199219 ) ;
#14754 = AXIS2_PLACEMENT_3D ( 'NONE', #14440, #13049, #14740 ) ;
#14755 = CARTESIAN_POINT ( 'NONE',  ( 30.00000000000000000, -122.0000000000000000, 2.099999999999991207 ) ) ;
#14756 = CARTESIAN_POINT ( 'NONE',  ( 19.99999999999999645, -49.77519642623978058, -42.18840861821836796 ) ) ;
#14757 = ORIENTED_EDGE ( 'NONE', *, *, #19033, .F. ) ;
#14758 =( GEOMETRIC_REPRESENTATION_CONTEXT ( 3 ) GLOBAL_UNCERTAINTY_ASSIGNED_CONTEXT ( ( #15558 ) ) GLOBAL_UNIT_ASSIGNED_CONTEXT ( ( #18543, #15555, #11958 ) ) REPRESENTATION_CONTEXT ( 'NONE', 'WORKASPACE' ) );
#14759 = DIRECTION ( 'NONE',  ( 0.000000000000000000, 0.000000000000000000, 1.000000000000000000 ) ) ;
#14760 = DIRECTION ( 'NONE',  ( 0.000000000000000000, 0.9976687691905394839, -0.06824241336466768670 ) ) ;
#14761 = DIRECTION ( 'NONE',  ( 0.000000000000000000, 0.000000000000000000, 1.000000000000000000 ) ) ;
#14762 = FACE_OUTER_BOUND ( 'NONE', #20586, .T. ) ;
#14763 = CARTESIAN_POINT ( 'NONE',  ( 19.99999999999999645, 64.36139404985964063, 32.27399814043896953 ) ) ;
#14764 = AXIS2_PLACEMENT_3D ( 'NONE', #11914, #10544, #3855 ) ;
#14765 = AXIS2_PLACEMENT_3D ( 'NONE', #17882, #165, #17975 ) ;
#14766 = ORIENTED_EDGE ( 'NONE', *, *, #12468, .T. ) ;
#14767 = CARTESIAN_POINT ( 'NONE',  ( 2.500000000000000000, -2.629050547790028551E-15, -2.041999999999999815 ) ) ;
#14768 = ORIENTED_EDGE ( 'NONE', *, *, #11943, .T. ) ;
#14769 = CARTESIAN_POINT ( 'NONE',  ( -6.232800000000000118, 0.000000000000000000, 0.000000000000000000 ) ) ;
#14770 = CARTESIAN_POINT ( 'NONE',  ( 21.00000000000000355, 0.000000000000000000, 0.000000000000000000 ) ) ;
#14771 = ORIENTED_EDGE ( 'NONE', *, *, #109, .F. ) ;
#14772 = EDGE_CURVE ( 'NONE', #7659, #13080, #19934, .T. ) ;
#14773 = CARTESIAN_POINT ( 'NONE',  ( 50.00100000000000477, -85.00000000000000000, -1.040949779275250179E-14 ) ) ;
#14774 = EDGE_LOOP ( 'NONE', ( #19840, #19770, #19487, #160 ) ) ;
#14775 = CARTESIAN_POINT ( 'NONE',  ( -30.00000000000000000, -85.00000000000000000, -1.040949779275250179E-14 ) ) ;
#14776 = EDGE_CURVE ( 'NONE', #10416, #18098, #18354, .T. ) ;
#14777 = AXIS2_PLACEMENT_3D ( 'NONE', #3705, #8692, #643 ) ;
#14778 = ORIENTED_EDGE ( 'NONE', *, *, #2233, .T. ) ;
#14779 = CIRCLE ( 'NONE', #19184, 27.60000000002760245 ) ;
#14780 = EDGE_CURVE ( 'NONE', #12132, #3634, #11296, .T. ) ;
#14781 = DIRECTION ( 'NONE',  ( -1.000000000000000000, -0.000000000000000000, -0.000000000000000000 ) ) ;
#14782 = AXIS2_PLACEMENT_3D ( 'NONE', #20205, #16604, #12055 ) ;
#14783 = VECTOR ( 'NONE', #10334, 1000.000000000000000 ) ;
#14784 = DIRECTION ( 'NONE',  ( -1.000000000000000000, 0.000000000000000000, 0.000000000000000000 ) ) ;
#14785 = CARTESIAN_POINT ( 'NONE',  ( -2.222972768810837607, 11.17563879758428769, 4.416828500647428157 ) ) ;
#14786 = ORIENTED_EDGE ( 'NONE', *, *, #20119, .F. ) ;
#14787 = DIRECTION ( 'NONE',  ( 0.000000000000000000, 0.8169698930104430934, -0.5766803221148655290 ) ) ;
#14788 = CIRCLE ( 'NONE', #8348, 2.041999999999999815 ) ;
#14789 = DIRECTION ( 'NONE',  ( 0.000000000000000000, 0.000000000000000000, -1.000000000000000000 ) ) ;
#14790 = EDGE_LOOP ( 'NONE', ( #12528, #9532, #6613 ) ) ;
#14791 = DIRECTION ( 'NONE',  ( 0.000000000000000000, 0.000000000000000000, 1.000000000000000000 ) ) ;
#14792 = EDGE_CURVE ( 'NONE', #4671, #20034, #812, .T. ) ;
#14793 = EDGE_LOOP ( 'NONE', ( #3904, #10102, #20401, #8748 ) ) ;
#14794 = CIRCLE ( 'NONE', #5644, 17.50000000000000355 ) ;
#14795 = CARTESIAN_POINT ( 'NONE',  ( -31.74999999999995737, 0.000000000000000000, 0.000000000000000000 ) ) ;
#14796 = DIRECTION ( 'NONE',  ( -1.000000000000000000, 0.000000000000000000, 0.000000000000000000 ) ) ;
#14797 = CARTESIAN_POINT ( 'NONE',  ( -6.177131623262581250, -10.85999999999999410, 1.329966423874025547E-15 ) ) ;
#14798 = EDGE_CURVE ( 'NONE', #10258, #10665, #14011, .T. ) ;
#14799 = AXIS2_PLACEMENT_3D ( 'NONE', #4321, #17146, #15759 ) ;
#14800 = ORIENTED_EDGE ( 'NONE', *, *, #14076, .T. ) ;
#14801 = AXIS2_PLACEMENT_3D ( 'NONE', #2655, #16182, #17172 ) ;
#14802 = EDGE_CURVE ( 'NONE', #8802, #13140, #14972, .T. ) ;
#14803 = FACE_BOUND ( 'NONE', #15890, .T. ) ;
#14804 = ORIENTED_EDGE ( 'NONE', *, *, #3891, .T. ) ;
#14805 =( LENGTH_UNIT ( ) NAMED_UNIT ( * ) SI_UNIT ( .MILLI., .METRE. ) );
#14806 = DIRECTION ( 'NONE',  ( -1.000000000000000000, -0.000000000000000000, -0.000000000000000000 ) ) ;
#14807 = EDGE_CURVE ( 'NONE', #10156, #8987, #4864, .T. ) ;
#14808 = AXIS2_PLACEMENT_3D ( 'NONE', #5708, #18131, #18555 ) ;
#14809 = ORIENTED_EDGE ( 'NONE', *, *, #13131, .T. ) ;
#14810 = CARTESIAN_POINT ( 'NONE',  ( 0.000000000000000000, 0.000000000000000000, -5.574599999999999334 ) ) ;
#14811 = VECTOR ( 'NONE', #6405, 1000.000000000000000 ) ;
#14812 = CARTESIAN_POINT ( 'NONE',  ( 19.99999999999999645, 64.52323195238628273, 6.389157729493382121 ) ) ;
#14813 = SHAPE_DEFINITION_REPRESENTATION ( #10708, #11016 ) ;
#14814 = CARTESIAN_POINT ( 'NONE',  ( -16.62983158437510411, 6.888301784570731279, -18.51488749981969306 ) ) ;
#14816 = ORIENTED_EDGE ( 'NONE', *, *, #5658, .T. ) ;
#14815 = AXIS2_PLACEMENT_3D ( 'NONE', #9045, #12329, #4268 ) ;
#14817 = CARTESIAN_POINT ( 'NONE',  ( -12.50000000000000533, 0.000000000000000000, 40.00000000000000000 ) ) ;
#14818 = EDGE_CURVE ( 'NONE', #5904, #19715, #18076, .T. ) ;
#14819 = EDGE_CURVE ( 'NONE', #11622, #17731, #16700, .T. ) ;
#14820 = CARTESIAN_POINT ( 'NONE',  ( -2.943691925285395694, 14.79893867793683349, -1.953573168480927214 ) ) ;
#14821 = ADVANCED_FACE ( 'NONE', ( #2145 ), #5218, .T. ) ;
#14822 = DIRECTION ( 'NONE',  ( -1.836909530733573776E-16, 1.000000000000000000, 0.000000000000000000 ) ) ;
#14823 = ORIENTED_EDGE ( 'NONE', *, *, #19059, .F. ) ;
#14824 = CARTESIAN_POINT ( 'NONE',  ( 4.999999999999997335, 0.000000000000000000, 0.000000000000000000 ) ) ;
#14825 = AXIS2_PLACEMENT_3D ( 'NONE', #19693, #5174, #10062 ) ;
#14826 = EDGE_CURVE ( 'NONE', #16392, #1061, #12676, .T. ) ;
#14827 = FACE_OUTER_BOUND ( 'NONE', #10391, .T. ) ;
#14828 = CARTESIAN_POINT ( 'NONE',  ( 30.11504063214072602, -46.04687138839951643, 66.48368087637908275 ) ) ;
#14829 = ORIENTED_EDGE ( 'NONE', *, *, #5333, .T. ) ;
#14830 = FACE_OUTER_BOUND ( 'NONE', #17787, .T. ) ;
#14831 = EDGE_LOOP ( 'NONE', ( #12540, #3402, #337, #7055 ) ) ;
#14832 = CARTESIAN_POINT ( 'NONE',  ( 19.99999999999999645, 0.000000000000000000, 0.000000000000000000 ) ) ;
#14833 = CARTESIAN_POINT ( 'NONE',  ( 24.74873734152916072, 24.74873734152916072, -130.0000000000000000 ) ) ;
#14834 = ORIENTED_EDGE ( 'NONE', *, *, #8419, .T. ) ;
#14835 = ORIENTED_EDGE ( 'NONE', *, *, #11424, .F. ) ;
#14836 = CARTESIAN_POINT ( 'NONE',  ( 19.99999999999999645, 6.872116855664026858, -64.47358224882410127 ) ) ;
#14837 = CARTESIAN_POINT ( 'NONE',  ( 19.99999999999999645, -64.52323195238632536, 6.389157729492951354 ) ) ;
#14838 = LINE ( 'NONE', #14935, #4479 ) ;
#14839 = DIRECTION ( 'NONE',  ( 0.000000000000000000, 0.000000000000000000, -1.000000000000000000 ) ) ;
#14840 = CARTESIAN_POINT ( 'NONE',  ( 4.000000000000000000, 0.000000000000000000, 0.000000000000000000 ) ) ;
#14841 = CARTESIAN_POINT ( 'NONE',  ( 2.870125741905214412, -6.929096494179682431, 17.83088750018031732 ) ) ;
#14842 = CARTESIAN_POINT ( 'NONE',  ( -6.330490858644137298, -9.474249097082495297, -6.240266000286802672 ) ) ;
#14843 = LINE ( 'NONE', #13048, #4022 ) ;
#14844 = CARTESIAN_POINT ( 'NONE',  ( -30.00000000000000000, -85.00000000000000000, 14.49999999999998579 ) ) ;
#14845 = EDGE_LOOP ( 'NONE', ( #7795, #13889 ) ) ;
#14846 = DIRECTION ( 'NONE',  ( -0.000000000000000000, 0.000000000000000000, -1.000000000000000000 ) ) ;
#14847 = CARTESIAN_POINT ( 'NONE',  ( -15.25966317163203279, -10.19618095047498052, 8.287456250180312622 ) ) ;
#14848 = CARTESIAN_POINT ( 'NONE',  ( -30.00000000000000000, -3.649167310370820871, 90.00000000000000000 ) ) ;
#14849 = VERTEX_POINT ( 'NONE', #13391 ) ;
#14850 = FACE_OUTER_BOUND ( 'NONE', #3551, .T. ) ;
#14851 = VERTEX_POINT ( 'NONE', #15075 ) ;
#14852 = CARTESIAN_POINT ( 'NONE',  ( 30.00000000000000000, -39.99999999999999289, -52.00000000000000000 ) ) ;
#14853 = CARTESIAN_POINT ( 'NONE',  ( 31.92289614601317282, -34.44341132653233473, -66.98101497439323282 ) ) ;
#14854 = EDGE_LOOP ( 'NONE', ( #1209, #3314, #1139, #7164 ) ) ;
#14855 = ORIENTED_EDGE ( 'NONE', *, *, #6286, .F. ) ;
#14856 = CARTESIAN_POINT ( 'NONE',  ( 24.99999999999999645, -30.00000000000000711, -1.040949779275250179E-14 ) ) ;
#14857 = EDGE_CURVE ( 'NONE', #19414, #5038, #20423, .T. ) ;
#14858 = EDGE_CURVE ( 'NONE', #12828, #20933, #18419, .T. ) ;
#14859 = FILL_AREA_STYLE ('',( #6897 ) ) ;
#14860 = CARTESIAN_POINT ( 'NONE',  ( 0.000000000000000000, 28.84646472442533494, -58.52617768068405013 ) ) ;
#14861 = B_SPLINE_CURVE_WITH_KNOTS ( 'NONE', 3,
 ( #11107, #12908, #3149, #16190 ),
 .UNSPECIFIED., .F., .F.,
 ( 4, 4 ),
 ( 2.380737581618758185E-07, 0.002336974151641576809 ),
 .UNSPECIFIED. ) ;
#14862 = PLANE ( 'NONE',  #13331 ) ;
#14863 = ORIENTED_EDGE ( 'NONE', *, *, #5202, .F. ) ;
#14864 = CARTESIAN_POINT ( 'NONE',  ( 7.500000000000000888, -9.015933403756337545E-10, 9.798800000180312608 ) ) ;
#14865 = CARTESIAN_POINT ( 'NONE',  ( 19.99999999999999645, 0.000000000000000000, 0.000000000000000000 ) ) ;
#14866 = DIRECTION ( 'NONE',  ( -0.000000000000000000, -0.000000000000000000, -1.000000000000000000 ) ) ;
#14867 = FACE_OUTER_BOUND ( 'NONE', #3995, .T. ) ;
#14868 = VERTEX_POINT ( 'NONE', #13604 ) ;
#14869 = CARTESIAN_POINT ( 'NONE',  ( 0.000000000000000000, 0.000000000000000000, 0.000000000000000000 ) ) ;
#14870 = ORIENTED_EDGE ( 'NONE', *, *, #4356, .F. ) ;
#14871 = CARTESIAN_POINT ( 'NONE',  ( 0.000000000000000000, 5.051668046482832750E-16, -4.000000000000000000 ) ) ;
#14872 = CARTESIAN_POINT ( 'NONE',  ( 0.000000000000000000, 36.59093685910711002, -62.00889726307995176 ) ) ;
#14873 = ORIENTED_EDGE ( 'NONE', *, *, #19370, .T. ) ;
#14874 = FACE_OUTER_BOUND ( 'NONE', #8428, .T. ) ;
#14875 = ORIENTED_EDGE ( 'NONE', *, *, #10070, .T. ) ;
#14876 = DIRECTION ( 'NONE',  ( 0.000000000000000000, 0.000000000000000000, -1.000000000000000000 ) ) ;
#14877 = FACE_BOUND ( 'NONE', #57, .T. ) ;
#14878 = EDGE_LOOP ( 'NONE', ( #8082, #16331, #10540, #19876, #18281, #10340 ) ) ;
#14879 = EDGE_CURVE ( 'NONE', #12782, #13834, #10977, .T. ) ;
#14880 = CYLINDRICAL_SURFACE ( 'NONE', #4661, 27.60000000002760245 ) ;
#14881 = DIRECTION ( 'NONE',  ( 0.000000000000000000, 0.000000000000000000, 1.000000000000000000 ) ) ;
#14882 = VECTOR ( 'NONE', #4059, 1000.000000000000000 ) ;
#14883 = DIRECTION ( 'NONE',  ( 0.000000000000000000, 0.000000000000000000, 1.000000000000000000 ) ) ;
#14884 = CARTESIAN_POINT ( 'NONE',  ( 11.17563879758428769, 2.222972768810838939, 6.773078500647428335 ) ) ;
#14885 = EDGE_CURVE ( 'NONE', #15935, #14689, #4164, .T. ) ;
#14886 = EDGE_CURVE ( 'NONE', #10522, #231, #16990, .T. ) ;
#14887 = VERTEX_POINT ( 'NONE', #10432 ) ;
#14888 = CARTESIAN_POINT ( 'NONE',  ( 50.00000000000000000, -97.49621075554985339, 111.6458212409894486 ) ) ;
#14889 = CARTESIAN_POINT ( 'NONE',  ( -6.680000000000000604, 11.50000000000000000, 0.000000000000000000 ) ) ;
#14890 = ORIENTED_EDGE ( 'NONE', *, *, #6716, .T. ) ;
#14891 = CYLINDRICAL_SURFACE ( 'NONE', #17605, 27.60000000002759535 ) ;
#14892 = ORIENTED_EDGE ( 'NONE', *, *, #1714, .T. ) ;
#14893 = CARTESIAN_POINT ( 'NONE',  ( 2.163825119083639534E-09, 18.00000000000000000, 2.102300000180311823 ) ) ;
#14894 = DIRECTION ( 'NONE',  ( -1.000000000000000000, -0.000000000000000000, -0.000000000000000000 ) ) ;
#14895 = DIRECTION ( 'NONE',  ( 0.000000000000000000, 0.000000000000000000, 1.000000000000000000 ) ) ;
#14896 = EDGE_CURVE ( 'NONE', #14401, #18469, #20378, .T. ) ;
#14897 = EDGE_LOOP ( 'NONE', ( #20295, #20529, #13975, #2865 ) ) ;
#14898 = CARTESIAN_POINT ( 'NONE',  ( 9.999999999999998224, 46.17500197033058384, 55.24372537266413730 ) ) ;
#14899 = ORIENTED_EDGE ( 'NONE', *, *, #4912, .T. ) ;
#14900 = LINE ( 'NONE', #13209, #4829 ) ;
#14901 = DIRECTION ( 'NONE',  ( -1.000000000000000000, 0.000000000000000000, 0.000000000000000000 ) ) ;
#14902 = CIRCLE ( 'NONE', #11185, 2.041999999999999815 ) ;
#14903 = VERTEX_POINT ( 'NONE', #2586 ) ;
#14904 = DIRECTION ( 'NONE',  ( 0.000000000000000000, 0.000000000000000000, 1.000000000000000000 ) ) ;
#14905 = PRODUCT_DEFINITION_SHAPE ( 'NONE', 'NONE',  #20947 ) ;
#14906 = CARTESIAN_POINT ( 'NONE',  ( -10.00000000000000000, 0.000000000000000000, 0.000000000000000000 ) ) ;
#14907 = APPLICATION_PROTOCOL_DEFINITION ( 'draft international standard', 'automotive_design', 1998, #2073 ) ;
#14908 = CARTESIAN_POINT ( 'NONE',  ( 2.943691925285398803, -14.79893867793684059, 8.377010668841545993 ) ) ;
#14909 = ADVANCED_FACE ( 'NONE', ( #15406 ), #4051, .T. ) ;
#14910 = ORIENTED_EDGE ( 'NONE', *, *, #2506, .F. ) ;
#14911 = EDGE_CURVE ( 'NONE', #17275, #16351, #10296, .T. ) ;
#14912 = CIRCLE ( 'NONE', #19296, 65.24900000006526568 ) ;
#14913 = DIRECTION ( 'NONE',  ( 0.000000000000000000, 0.000000000000000000, -1.000000000000000000 ) ) ;
#14914 = ORIENTED_EDGE ( 'NONE', *, *, #2211, .F. ) ;
#14915 = CARTESIAN_POINT ( 'NONE',  ( 0.000000000000000000, 0.000000000000000000, 0.000000000000000000 ) ) ;
#14916 = CARTESIAN_POINT ( 'NONE',  ( -3.580422610670017658, 18.00000000043040771, 18.75316875018031126 ) ) ;
#14917 = AXIS2_PLACEMENT_3D ( 'NONE', #8602, #760, #869 ) ;
#14918 = VERTEX_POINT ( 'NONE', #16781 ) ;
#14919 = EDGE_CURVE ( 'NONE', #3519, #10526, #2172, .T. ) ;
#14920 = AXIS2_PLACEMENT_3D ( 'NONE', #122, #19302, #13163 ) ;
#14921 = ADVANCED_FACE ( 'NONE', ( #8938 ), #15294, .T. ) ;
#14922 = ORIENTED_EDGE ( 'NONE', *, *, #6195, .F. ) ;
#14923 = DIRECTION ( 'NONE',  ( -1.000000000000000000, -0.000000000000000000, -0.000000000000000000 ) ) ;
#14924 = LINE ( 'NONE', #10255, #1944 ) ;
#14925 = EDGE_LOOP ( 'NONE', ( #2331, #18426, #4949, #4213 ) ) ;
#14926 = EDGE_LOOP ( 'NONE', ( #487, #17639 ) ) ;
#14927 = PLANE ( 'NONE',  #19672 ) ;
#14928 = CARTESIAN_POINT ( 'NONE',  ( -17.99999999999999645, 2.163826221265758470E-09, -2.158549999819691312 ) ) ;
#14929 = ORIENTED_EDGE ( 'NONE', *, *, #1490, .F. ) ;
#14930 = EDGE_CURVE ( 'NONE', #1857, #11867, #5545, .T. ) ;
#14931 = ORIENTED_EDGE ( 'NONE', *, *, #7003, .F. ) ;
#14932 = CARTESIAN_POINT ( 'NONE',  ( 47.05877748208924061, -6.233954241158976117, -80.06349855976149854 ) ) ;
#14933 = EDGE_CURVE ( 'NONE', #14851, #1850, #14611, .T. ) ;
#14934 = CARTESIAN_POINT ( 'NONE',  ( -11.50000000000000000, 1.408343819019456176E-15, 68.00000000000000000 ) ) ;
#14935 = CARTESIAN_POINT ( 'NONE',  ( 10.00000000000000178, -148.4917293642369884, -48.67032260359990659 ) ) ;
#14936 = CIRCLE ( 'NONE', #13928, 27.60000000002759535 ) ;
#14937 = SURFACE_STYLE_FILL_AREA ( #13040 ) ;
#14938 = CARTESIAN_POINT ( 'NONE',  ( 15.25966317163203101, 10.19618095047498585, 22.42495625018030836 ) ) ;
#14939 = UNCERTAINTY_MEASURE_WITH_UNIT (LENGTH_MEASURE( 1.000000000000000082E-05 ), #5009, 'distance_accuracy_value', 'NONE');
#14940 = ADVANCED_FACE ( 'NONE', ( #13827 ), #7124, .T. ) ;
#14941 = CARTESIAN_POINT ( 'NONE',  ( 30.00000000000000000, -148.4917293642369600, 48.67032260359987816 ) ) ;
#14942 = CARTESIAN_POINT ( 'NONE',  ( 5.303300859536635770, 5.303300858261589923, 14.88557500018031554 ) ) ;
#14943 = CARTESIAN_POINT ( 'NONE',  ( -11.17563879731704723, 1.343452237168308679E-09, 4.657390249713198926 ) ) ;
#14944 = DIRECTION ( 'NONE',  ( -1.000000000000000000, -0.000000000000000000, 0.000000000000000000 ) ) ;
#14945 = CARTESIAN_POINT ( 'NONE',  ( 50.00000000000000000, 36.35083268962920044, -90.00000000000000000 ) ) ;
#14946 = AXIS2_PLACEMENT_3D ( 'NONE', #11236, #314, #8067 ) ;
#14947 = AXIS2_PLACEMENT_3D ( 'NONE', #12373, #4317, #10785 ) ;
#14948 = ORIENTED_EDGE ( 'NONE', *, *, #986, .T. ) ;
#14949 = DIRECTION ( 'NONE',  ( -1.000000000000000000, 0.000000000000000000, 0.000000000000000000 ) ) ;
#14950 = CARTESIAN_POINT ( 'NONE',  ( 16.62983158603122291, 6.888301780572502864, 22.71948750018031404 ) ) ;
#14951 = FACE_OUTER_BOUND ( 'NONE', #20627, .T. ) ;
#14952 = AXIS2_PLACEMENT_3D ( 'NONE', #14832, #8250, #3470 ) ;
#14953 = EDGE_LOOP ( 'NONE', ( #12149, #17298, #16173, #3084 ) ) ;
#14954 = DIRECTION ( 'NONE',  ( 0.000000000000000000, 0.000000000000000000, 1.000000000000000000 ) ) ;
#14955 = EDGE_LOOP ( 'NONE', ( #3463, #12980, #927, #11508, #9692, #13513, #7482, #10628, #4900, #19610, #9042, #17568 ) ) ;
#14956 = DIRECTION ( 'NONE',  ( 1.000000000000000000, -0.000000000000000000, -0.000000000000000000 ) ) ;
#14957 = CARTESIAN_POINT ( 'NONE',  ( 2.000000000000010658, -3.464101615137748169, -5.600000000000000533 ) ) ;
#14958 = VERTEX_POINT ( 'NONE', #8618 ) ;
#14959 = AXIS2_PLACEMENT_3D ( 'NONE', #9341, #12745, #7751 ) ;
#14960 = EDGE_LOOP ( 'NONE', ( #5819, #8148, #6353, #11603 ) ) ;
#14961 = DIRECTION ( 'NONE',  ( -0.000000000000000000, -0.000000000000000000, 1.000000000000000000 ) ) ;
#14962 = EDGE_CURVE ( 'NONE', #13015, #6246, #4196, .T. ) ;
#14963 = LINE ( 'NONE', #8281, #4210 ) ;
#14964 = CIRCLE ( 'NONE', #5812, 2.649999999999994582 ) ;
#14965 = VECTOR ( 'NONE', #17723, 1000.000000000000000 ) ;
#14966 = CARTESIAN_POINT ( 'NONE',  ( 0.000000000000000000, 55.05624179292029652, -35.01774179823726740 ) ) ;
#14967 = VECTOR ( 'NONE', #12929, 1000.000000000000000 ) ;
#14968 = FACE_OUTER_BOUND ( 'NONE', #8317, .T. ) ;
#14969 = FACE_OUTER_BOUND ( 'NONE', #10448, .T. ) ;
#14970 =( NAMED_UNIT ( * ) PLANE_ANGLE_UNIT ( ) SI_UNIT ( $, .RADIAN. ) );
#14971 = PLANE ( 'NONE',  #12902 ) ;
#14972 = LINE ( 'NONE', #560, #16374 ) ;
#14973 = ORIENTED_EDGE ( 'NONE', *, *, #3834, .F. ) ;
#14974 = EDGE_CURVE ( 'NONE', #8586, #6927, #711, .T. ) ;
#14975 = DIRECTION ( 'NONE',  ( 0.000000000000000000, 0.000000000000000000, 1.000000000000000000 ) ) ;
#14976 = ORIENTED_EDGE ( 'NONE', *, *, #13882, .T. ) ;
#14977 = DIRECTION ( 'NONE',  ( -1.000000000000000000, -0.000000000000000000, 0.000000000000000000 ) ) ;
#14978 = CARTESIAN_POINT ( 'NONE',  ( -19.81419003091921383, -8.351337688303456019, 78.32518794914261662 ) ) ;
#14979 = EDGE_LOOP ( 'NONE', ( #15156, #6395, #19527 ) ) ;
#14980 = CIRCLE ( 'NONE', #17344, 27.60000000002761311 ) ;
#14981 = LINE ( 'NONE', #16772, #5868 ) ;
#14982 = ORIENTED_EDGE ( 'NONE', *, *, #4044, .F. ) ;
#14983 = DIRECTION ( 'NONE',  ( 0.000000000000000000, 0.000000000000000000, -1.000000000000000000 ) ) ;
#14984 = DIRECTION ( 'NONE',  ( -0.000000000000000000, -0.000000000000000000, 1.000000000000000000 ) ) ;
#14985 = ORIENTED_EDGE ( 'NONE', *, *, #8593, .F. ) ;
#14986 = AXIS2_PLACEMENT_3D ( 'NONE', #12148, #18408, #387 ) ;
#14987 = DIRECTION ( 'NONE',  ( 0.000000000000000000, 0.000000000000000000, -1.000000000000000000 ) ) ;
#14988 = CARTESIAN_POINT ( 'NONE',  ( -3.580422610670017658, 18.00000000043040771, -9.521831249819690868 ) ) ;
#14989 = DIRECTION ( 'NONE',  ( -1.000000000000000000, 0.000000000000000000, 0.000000000000000000 ) ) ;
#14990 = CYLINDRICAL_SURFACE ( 'NONE', #4508, 72.00000000007199219 ) ;
#14991 = CARTESIAN_POINT ( 'NONE',  ( -6.330490856366295382, 9.474249098604511587, 13.25276600064742993 ) ) ;
#14992 = AXIS2_PLACEMENT_3D ( 'NONE', #14487, #1245, #7698 ) ;
#14994 = VERTEX_POINT ( 'NONE', #12337 ) ;
#14993 = CIRCLE ( 'NONE', #3792, 65.24900000006526568 ) ;
#14995 = FACE_OUTER_BOUND ( 'NONE', #712, .T. ) ;
#14996 = ORIENTED_EDGE ( 'NONE', *, *, #2654, .F. ) ;
#14997 = CARTESIAN_POINT ( 'NONE',  ( 19.99999999999999645, 0.000000000000000000, 0.000000000000000000 ) ) ;
#14998 = VERTEX_POINT ( 'NONE', #18804 ) ;
#14999 = EDGE_CURVE ( 'NONE', #17243, #7832, #5647, .T. ) ;
#15000 = CARTESIAN_POINT ( 'NONE',  ( -12.72792205982779912, 12.72792206288790950, 0.9241750001803133996 ) ) ;
#15001 = DIRECTION ( 'NONE',  ( -1.508455196501572169E-16, 1.000000000000000000, 0.000000000000000000 ) ) ;
#15002 = FACE_OUTER_BOUND ( 'NONE', #4683, .T. ) ;
#15003 = AXIS2_PLACEMENT_3D ( 'NONE', #1334, #20808, #12780 ) ;
#15004 = AXIS2_PLACEMENT_3D ( 'NONE', #6256, #12306, #9334 ) ;
#15005 = ORIENTED_EDGE ( 'NONE', *, *, #16443, .T. ) ;
#15006 = DIRECTION ( 'NONE',  ( 0.000000000000000000, -1.000000000000000000, 0.000000000000000000 ) ) ;
#15007 = EDGE_LOOP ( 'NONE', ( #8098, #18476, #10051, #7331, #8687, #11342 ) ) ;
#15008 = VECTOR ( 'NONE', #19755, 1000.000000000000000 ) ;
#15009 = EDGE_CURVE ( 'NONE', #10935, #7472, #17755, .T. ) ;
#15010 = DIRECTION ( 'NONE',  ( -1.000000000000000000, 0.000000000000000000, 0.000000000000000000 ) ) ;
#15011 = CIRCLE ( 'NONE', #8906, 72.00000000007199219 ) ;
#15012 = EDGE_LOOP ( 'NONE', ( #1297, #5776, #8075, #16692 ) ) ;
#15013 = DIRECTION ( 'NONE',  ( 1.000000000000000000, 0.000000000000000000, -0.000000000000000000 ) ) ;
#15014 = DIRECTION ( 'NONE',  ( -1.000000000000000000, -0.000000000000000000, -0.000000000000000000 ) ) ;
#15015 = APPLICATION_PROTOCOL_DEFINITION ( 'draft international standard', 'automotive_design', 1998, #4657 ) ;
#15016 = AXIS2_PLACEMENT_3D ( 'NONE', #5105, #1542, #16250 ) ;
#15017 = CARTESIAN_POINT ( 'NONE',  ( 13.67243654778935991, 5.663308646854338768, 15.15122941884154883 ) ) ;
#15018 = AXIS2_PLACEMENT_3D ( 'NONE', #4879, #11349, #6668 ) ;
#15019 = VECTOR ( 'NONE', #5015, 1000.000000000000000 ) ;
#15020 = EDGE_LOOP ( 'NONE', ( #5266, #10811, #13878, #17285 ) ) ;
#15021 = DIRECTION ( 'NONE',  ( -1.000000000000000000, 0.000000000000000000, 0.000000000000000000 ) ) ;
#15022 = CIRCLE ( 'NONE', #4523, 27.60000000002759535 ) ;
#15023 = CIRCLE ( 'NONE', #13005, 2.649999999999999467 ) ;
#15024 = CARTESIAN_POINT ( 'NONE',  ( 2.943691925285397470, -14.79893867793683349, -16.09107316848092140 ) ) ;
#15025 = AXIS2_PLACEMENT_3D ( 'NONE', #4290, #1126, #15938 ) ;
#15026 = LINE ( 'NONE', #16713, #19009 ) ;
#15027 = ORIENTED_EDGE ( 'NONE', *, *, #3343, .T. ) ;
#15028 = DIRECTION ( 'NONE',  ( 1.000000000000000000, 0.000000000000000000, 0.000000000000000000 ) ) ;
#15029 = CARTESIAN_POINT ( 'NONE',  ( 39.99999999999997158, -122.3205080756887497, -80.28096411455980785 ) ) ;
#15030 = CIRCLE ( 'NONE', #14035, 2.649999999999987477 ) ;
#15031 = VERTEX_POINT ( 'NONE', #14147 ) ;
#15032 = ADVANCED_FACE ( 'NONE', ( #4698 ), #19121, .T. ) ;
#15033 = DIRECTION ( 'NONE',  ( -1.000000000000000000, -0.000000000000000000, -0.000000000000000000 ) ) ;
#15034 = ORIENTED_EDGE ( 'NONE', *, *, #4725, .F. ) ;
#15035 = CARTESIAN_POINT ( 'NONE',  ( 0.000000000000000000, 0.000000000000000000, 0.000000000000000000 ) ) ;
#15036 = CARTESIAN_POINT ( 'NONE',  ( 16.62983158437509346, -6.888301784570737496, 3.143012500180311086 ) ) ;
#15037 = EDGE_CURVE ( 'NONE', #6083, #8981, #11986, .T. ) ;
#15038 = ORIENTED_EDGE ( 'NONE', *, *, #14677, .T. ) ;
#15039 = ORIENTED_EDGE ( 'NONE', *, *, #7940, .T. ) ;
#15040 = DIRECTION ( 'NONE',  ( -1.000000000000000000, 0.000000000000000000, 0.000000000000000000 ) ) ;
#15041 = VECTOR ( 'NONE', #19109, 1000.000000000000000 ) ;
#15042 = CARTESIAN_POINT ( 'NONE',  ( -9.850000000000019185, 3.245314017740474129E-16, 166.0000000000000000 ) ) ;
#15043 = DIRECTION ( 'NONE',  ( -0.000000000000000000, -0.000000000000000000, -1.000000000000000000 ) ) ;
#15044 = ADVANCED_FACE ( 'NONE', ( #12545 ), #7923, .T. ) ;
#15045 = CARTESIAN_POINT ( 'NONE',  ( -3.580422610670018990, 18.00000000043041481, 20.65776875018030978 ) ) ;
#15046 = DIRECTION ( 'NONE',  ( 0.000000000000000000, 0.000000000000000000, -1.000000000000000000 ) ) ;
#15047 = CARTESIAN_POINT ( 'NONE',  ( 6.358192987158595599, -4.248408730893249441, 7.522293750180316430 ) ) ;
#15048 = CARTESIAN_POINT ( 'NONE',  ( 4.276731812588566939, -10.32494394809438809, -17.13792225028680249 ) ) ;
#15049 = DIRECTION ( 'NONE',  ( 0.000000000000000000, 0.000000000000000000, -1.000000000000000000 ) ) ;
#15050 = CARTESIAN_POINT ( 'NONE',  ( 52.50000000000000000, -40.00000000000000000, 5.000000000000000000 ) ) ;
#15051 = EDGE_CURVE ( 'NONE', #19712, #6167, #5225, .T. ) ;
#15052 = AXIS2_PLACEMENT_3D ( 'NONE', #1916, #16133, #3393 ) ;
#15053 = VERTEX_POINT ( 'NONE', #1420 ) ;
#15054 = DIRECTION ( 'NONE',  ( 0.000000000000000000, 0.000000000000000000, -1.000000000000000000 ) ) ;
#15055 = CARTESIAN_POINT ( 'NONE',  ( 3.580422610670020322, -18.00000000043041126, -2.904731249819686223 ) ) ;
#15056 = FACE_BOUND ( 'NONE', #12282, .T. ) ;
#15057 = ORIENTED_EDGE ( 'NONE', *, *, #17626, .T. ) ;
#15058 = ADVANCED_FACE ( 'NONE', ( #7874 ), #2898, .F. ) ;
#15059 = DIRECTION ( 'NONE',  ( 1.000000000000000000, 0.000000000000000000, 0.000000000000000000 ) ) ;
#15060 = ORIENTED_EDGE ( 'NONE', *, *, #5355, .F. ) ;
#15061 = CARTESIAN_POINT ( 'NONE',  ( 24.99999999999999645, -39.99999999999999289, 49.89999999999999858 ) ) ;
#15062 = CARTESIAN_POINT ( 'NONE',  ( 0.000000000000000000, -64.36139404985986801, 32.27399814043853610 ) ) ;
#15063 = EDGE_CURVE ( 'NONE', #10906, #7485, #485, .T. ) ;
#15064 = ORIENTED_EDGE ( 'NONE', *, *, #824, .F. ) ;
#15065 = ORIENTED_EDGE ( 'NONE', *, *, #18611, .T. ) ;
#15066 = AXIS2_PLACEMENT_3D ( 'NONE', #2843, #7726, #4540 ) ;
#15067 = CARTESIAN_POINT ( 'NONE',  ( 50.00000000000000000, -97.49621075554985339, 111.6458212409894486 ) ) ;
#15068 = EDGE_CURVE ( 'NONE', #1492, #701, #2851, .T. ) ;
#15069 = DIRECTION ( 'NONE',  ( 0.000000000000000000, 0.000000000000000000, 1.000000000000000000 ) ) ;
#15070 = AXIS2_PLACEMENT_3D ( 'NONE', #19341, #6094, #9705 ) ;
#15071 = DIRECTION ( 'NONE',  ( 0.000000000000000000, 0.000000000000000000, -1.000000000000000000 ) ) ;
#15072 = CARTESIAN_POINT ( 'NONE',  ( 6.358192988180013216, 4.248408729364577141, -0.5097937498196903894 ) ) ;
#15073 = DIRECTION ( 'NONE',  ( 0.000000000000000000, 0.000000000000000000, -1.000000000000000000 ) ) ;
#15074 = CARTESIAN_POINT ( 'NONE',  ( 0.000000000000000000, -63.17103598352115057, -16.33561182745204476 ) ) ;
#15075 = CARTESIAN_POINT ( 'NONE',  ( 30.00000000000000000, -50.00000000000000000, -66.88656633939928042 ) ) ;
#15076 = ADVANCED_FACE ( 'NONE', ( #7664 ), #14242, .F. ) ;
#15077 = ORIENTED_EDGE ( 'NONE', *, *, #17774, .T. ) ;
#15078 = DIRECTION ( 'NONE',  ( 0.000000000000000000, 0.000000000000000000, 1.000000000000000000 ) ) ;
#15079 = EDGE_LOOP ( 'NONE', ( #4311, #6662, #11367, #2743 ) ) ;
#15080 = CARTESIAN_POINT ( 'NONE',  ( 3.580422614997668340, 17.99999999956958519, 0.4922312501803131624 ) ) ;
#15081 = CARTESIAN_POINT ( 'NONE',  ( 2.601994274788632211, -21.34541601844983916, 70.64469287327099778 ) ) ;
#15082 = ORIENTED_EDGE ( 'NONE', *, *, #3767, .F. ) ;
#15083 = DIRECTION ( 'NONE',  ( 0.000000000000000000, 1.000000000000000000, -1.287488025362403787E-15 ) ) ;
#15084 = ORIENTED_EDGE ( 'NONE', *, *, #16101, .F. ) ;
#15085 = PRODUCT_DEFINITION_SHAPE ( 'NONE', 'NONE',  #20954 ) ;
#15086 = LINE ( 'NONE', #2465, #9505 ) ;
#15087 = CARTESIAN_POINT ( 'NONE',  ( 2.500000000000000000, 0.000000000000000000, 0.000000000000000000 ) ) ;
#15088 = EDGE_CURVE ( 'NONE', #13182, #1857, #10951, .T. ) ;
#15089 = ORIENTED_EDGE ( 'NONE', *, *, #16958, .T. ) ;
#15090 = DIRECTION ( 'NONE',  ( -1.000000000000000000, 0.000000000000000000, 0.000000000000000000 ) ) ;
#15091 = CARTESIAN_POINT ( 'NONE',  ( -6.888301780572500199, 16.62983158603121936, -0.3913624998196918447 ) ) ;
#15092 = DIRECTION ( 'NONE',  ( -0.000000000000000000, -0.000000000000000000, -1.000000000000000000 ) ) ;
#15093 = EDGE_CURVE ( 'NONE', #5012, #1717, #15827, .T. ) ;
#15094 = DIRECTION ( 'NONE',  ( -0.000000000000000000, -0.000000000000000000, 1.000000000000000000 ) ) ;
#15095 = CARTESIAN_POINT ( 'NONE',  ( 10.32494394809439875, 4.276731812588567827, 6.478547250647427980 ) ) ;
#15096 = B_SPLINE_CURVE_WITH_KNOTS ( 'NONE', 3,
 ( #16339, #1829, #3317, #6583 ),
 .UNSPECIFIED., .F., .F.,
 ( 4, 4 ),
 ( 2.380737581781750353E-07, 0.002336974151641521731 ),
 .UNSPECIFIED. ) ;
#15097 = ORIENTED_EDGE ( 'NONE', *, *, #5089, .F. ) ;
#15098 = AXIS2_PLACEMENT_3D ( 'NONE', #17974, #3442, #4936 ) ;
#15099 = VECTOR ( 'NONE', #4363, 1000.000000000000000 ) ;
#15100 = CARTESIAN_POINT ( 'NONE',  ( 12.92641286132474931, -1.553915700095510638E-09, 25.24826151322289647 ) ) ;
#15101 = EDGE_LOOP ( 'NONE', ( #18759, #15683 ) ) ;
#15102 = DIRECTION ( 'NONE',  ( -1.000000000000000000, 0.000000000000000000, -0.000000000000000000 ) ) ;
#15103 = ORIENTED_EDGE ( 'NONE', *, *, #8065, .F. ) ;
#15104 = CARTESIAN_POINT ( 'NONE',  ( -16.62983158437510056, 6.888301784570729502, 0.3351125001803123560 ) ) ;
#15105 = AXIS2_PLACEMENT_3D ( 'NONE', #5527, #15400, #12330 ) ;
#15106 = CARTESIAN_POINT ( 'NONE',  ( 10.00000000000000178, -164.9999999999999716, -70.00000000000000000 ) ) ;
#15107 = DIRECTION ( 'NONE',  ( -1.000000000000000000, 0.000000000000000000, 0.000000000000000000 ) ) ;
#15108 = ORIENTED_EDGE ( 'NONE', *, *, #4679, .F. ) ;
#15109 = AXIS2_PLACEMENT_3D ( 'NONE', #16646, #16956, #18565 ) ;
#15110 = ORIENTED_EDGE ( 'NONE', *, *, #6598, .T. ) ;
#15111 = CARTESIAN_POINT ( 'NONE',  ( 1.040949779275250179E-14, -85.00000000000000000, 5.000000000000000000 ) ) ;
#15112 = AXIS2_PLACEMENT_3D ( 'NONE', #19180, #9432, #13994 ) ;
#15113 = AXIS2_PLACEMENT_3D ( 'NONE', #14590, #18187, #13312 ) ;
#15114 = ORIENTED_EDGE ( 'NONE', *, *, #8846, .F. ) ;
#15115 = CARTESIAN_POINT ( 'NONE',  ( 19.99999999999999645, 19.38316218894295417, -61.87375713200968619 ) ) ;
#15116 = EDGE_CURVE ( 'NONE', #7136, #1316, #6238, .T. ) ;
#15117 = EDGE_CURVE ( 'NONE', #2692, #3661, #2792, .T. ) ;
#15118 = AXIS2_PLACEMENT_3D ( 'NONE', #2891, #20900, #1102 ) ;
#15119 = DIRECTION ( 'NONE',  ( 0.000000000000000000, 0.000000000000000000, -1.000000000000000000 ) ) ;
#15120 = ITEM_DEFINED_TRANSFORMATION ( 'NONE', 'NONE', #7255,  #12461 ) ;
#15121 = CARTESIAN_POINT ( 'NONE',  ( -13.67243654778936168, -5.663308646854336992, 10.43872941884154493 ) ) ;
#15122 = ORIENTED_EDGE ( 'NONE', *, *, #18433, .T. ) ;
#15123 = AXIS2_PLACEMENT_3D ( 'NONE', #8062, #3286, #14625 ) ;
#15124 = CARTESIAN_POINT ( 'NONE',  ( 0.000000000000000000, 0.000000000000000000, -5.294516984716111097 ) ) ;
#15125 = DIRECTION ( 'NONE',  ( 0.000000000000000000, 0.000000000000000000, 1.000000000000000000 ) ) ;
#15126 = AXIS2_PLACEMENT_3D ( 'NONE', #2466, #10024, #9145 ) ;
#15127 = CARTESIAN_POINT ( 'NONE',  ( -12.54593441764187034, -8.382925368423267187, -23.74888566848093774 ) ) ;
#15128 = DIRECTION ( 'NONE',  ( 0.000000000000000000, -0.1361666490962330778, -0.9906859460363326431 ) ) ;
#15129 = ORIENTED_EDGE ( 'NONE', *, *, #3012, .T. ) ;
#15130 = CARTESIAN_POINT ( 'NONE',  ( 0.000000000000000000, 0.000000000000000000, 0.000000000000000000 ) ) ;
#15131 = CARTESIAN_POINT ( 'NONE',  ( 0.000000000000000000, -64.79224928664389438, -2.456263514198281150 ) ) ;
#15132 = AXIS2_PLACEMENT_3D ( 'NONE', #18235, #2329, #2430 ) ;
#15133 = ORIENTED_EDGE ( 'NONE', *, *, #17892, .T. ) ;
#15134 = ORIENTED_EDGE ( 'NONE', *, *, #19126, .F. ) ;
#15135 = DIRECTION ( 'NONE',  ( 0.000000000000000000, 0.000000000000000000, 1.000000000000000000 ) ) ;
#15136 = CARTESIAN_POINT ( 'NONE',  ( -10.19618095414378445, -15.25966316918061239, 5.793793750180310731 ) ) ;
#15137 = CIRCLE ( 'NONE', #16817, 17.00000000000002842 ) ;
#15138 = ORIENTED_EDGE ( 'NONE', *, *, #19552, .T. ) ;
#15139 = ORIENTED_EDGE ( 'NONE', *, *, #6078, .T. ) ;
#15140 = CARTESIAN_POINT ( 'NONE',  ( 47.99913302141636251, -4.465704580667236634, -88.98724172780555364 ) ) ;
#15141 = AXIS2_PLACEMENT_3D ( 'NONE', #17209, #15602, #3748 ) ;
#15142 = AXIS2_PLACEMENT_3D ( 'NONE', #16530, #19810, #11763 ) ;
#15143 = CARTESIAN_POINT ( 'NONE',  ( 19.99999999999999645, 0.000000000000000000, 0.000000000000000000 ) ) ;
#15144 = CARTESIAN_POINT ( 'NONE',  ( 0.000000000000000000, 0.000000000000000000, 166.0000000000000000 ) ) ;
#15145 = CARTESIAN_POINT ( 'NONE',  ( 6.888301784570730391, 16.62983158437510411, 21.54136250018031262 ) ) ;
#15146 = UNCERTAINTY_MEASURE_WITH_UNIT (LENGTH_MEASURE( 1.000000000000000082E-05 ), #18068, 'distance_accuracy_value', 'NONE');
#15147 = CARTESIAN_POINT ( 'NONE',  ( -9.015947181032835626E-10, -7.500000000000007994, -0.4300499998196871676 ) ) ;
#15148 = AXIS2_PLACEMENT_3D ( 'NONE', #2633, #826, #15650 ) ;
#15149 = EDGE_CURVE ( 'NONE', #18964, #7766, #9260, .T. ) ;
#15150 = EDGE_CURVE ( 'NONE', #16949, #9402, #15030, .T. ) ;
#15151 = CARTESIAN_POINT ( 'NONE',  ( 10.32494394706615637, -4.276731815070946574, -18.31604725028681102 ) ) ;
#15152 = AXIS2_PLACEMENT_3D ( 'NONE', #20711, #14063, #10671 ) ;
#15153 = DIRECTION ( 'NONE',  ( 1.000000000000000000, 0.000000000000000000, 0.000000000000000000 ) ) ;
#15154 = CARTESIAN_POINT ( 'NONE',  ( 9.999999999999998224, -10.74906464462068456, -71.19310085447979475 ) ) ;
#15155 = CIRCLE ( 'NONE', #6023, 11.49999999999999467 ) ;
#15156 = ORIENTED_EDGE ( 'NONE', *, *, #8842, .T. ) ;
#15157 = CYLINDRICAL_SURFACE ( 'NONE', #10223, 65.24900000006525147 ) ;
#15158 = CARTESIAN_POINT ( 'NONE',  ( -12.72792205982779912, 12.72792206288790950, 0.9241750001803133996 ) ) ;
#15159 = DIRECTION ( 'NONE',  ( 0.000000000000000000, 0.000000000000000000, 1.000000000000000000 ) ) ;
#15160 = ORIENTED_EDGE ( 'NONE', *, *, #2081, .T. ) ;
#15161 = EDGE_CURVE ( 'NONE', #4150, #2016, #17425, .T. ) ;
#15162 = CARTESIAN_POINT ( 'NONE',  ( 50.00000000000000000, -42.57363661491096707, 121.3828884801879155 ) ) ;
#15163 = ORIENTED_EDGE ( 'NONE', *, *, #17982, .F. ) ;
#15164 = CARTESIAN_POINT ( 'NONE',  ( 6.249999999999902300, -10.82531754730554496, 46.00000000000000711 ) ) ;
#15165 = CARTESIAN_POINT ( 'NONE',  ( 0.000000000000000000, 0.000000000000000000, 0.000000000000000000 ) ) ;
#15166 = ORIENTED_EDGE ( 'NONE', *, *, #10921, .F. ) ;
#15167 = ORIENTED_EDGE ( 'NONE', *, *, #14275, .F. ) ;
#15168 = DIRECTION ( 'NONE',  ( -0.000000000000000000, -0.000000000000000000, 1.000000000000000000 ) ) ;
#15169 =( NAMED_UNIT ( * ) SI_UNIT ( $, .STERADIAN. ) SOLID_ANGLE_UNIT ( ) );
#15170 = DIRECTION ( 'NONE',  ( 0.000000000000000000, 0.000000000000000000, -1.000000000000000000 ) ) ;
#15171 = CARTESIAN_POINT ( 'NONE',  ( 19.99999999999999645, 70.68211945903189530, 13.71269443944231980 ) ) ;
#15172 = ADVANCED_FACE ( 'NONE', ( #3102 ), #1534, .T. ) ;
#15173 = CARTESIAN_POINT ( 'NONE',  ( -7.499999999820661678, 1.491842756249031288, -13.46916874981968881 ) ) ;
#15174 = EDGE_CURVE ( 'NONE', #16423, #19553, #20795, .T. ) ;
#15175 = LINE ( 'NONE', #10190, #5408 ) ;
#15176 = CARTESIAN_POINT ( 'NONE',  ( 19.99999999999999645, -45.48683723007244595, 46.78012013466202035 ) ) ;
#15177 = CARTESIAN_POINT ( 'NONE',  ( 4.000000000000003553, 2.309401076758524685, -5.242734410091827613 ) ) ;
#15178 = DIRECTION ( 'NONE',  ( -1.000000000000000000, 0.000000000000000000, 0.000000000000000000 ) ) ;
#15179 = ORIENTED_EDGE ( 'NONE', *, *, #7961, .T. ) ;
#15180 = LINE ( 'NONE', #6908, #4796 ) ;
#15181 = VERTEX_POINT ( 'NONE', #5098 ) ;
#15182 = ADVANCED_FACE ( 'NONE', ( #8090 ), #9872, .T. ) ;
#15183 = CARTESIAN_POINT ( 'NONE',  ( 17.99999999956958163, -3.580422614997676334, 12.27348125018031411 ) ) ;
#15184 = CARTESIAN_POINT ( 'NONE',  ( -17.67520963998170203, -12.31071423659304109, 75.43714694428801693 ) ) ;
#15185 = VERTEX_POINT ( 'NONE', #6693 ) ;
#15186 = CARTESIAN_POINT ( 'NONE',  ( -7.500000000000000000, 0.000000000000000000, 40.00000000000000000 ) ) ;
#15187 = ORIENTED_EDGE ( 'NONE', *, *, #13240, .T. ) ;
#15188 = CARTESIAN_POINT ( 'NONE',  ( 6.249999999999902300, -10.82531754730554496, 166.0000000000000000 ) ) ;
#15189 = CARTESIAN_POINT ( 'NONE',  ( 6.249999999999902300, -10.82531754730554496, 129.0000000000000000 ) ) ;
#15190 = ORIENTED_EDGE ( 'NONE', *, *, #11530, .F. ) ;
#15191 = EDGE_CURVE ( 'NONE', #10498, #17301, #1845, .T. ) ;
#15192 = DIRECTION ( 'NONE',  ( 1.000000000000000000, 0.000000000000000000, 0.000000000000000000 ) ) ;
#15193 = CARTESIAN_POINT ( 'NONE',  ( 15.25966316918061239, -10.19618095414378445, -15.41245624981969087 ) ) ;
#15194 = DIRECTION ( 'NONE',  ( -1.000000000000000000, 0.000000000000000000, 0.000000000000000000 ) ) ;
#15195 = EDGE_CURVE ( 'NONE', #13187, #7518, #9621, .T. ) ;
#15196 = CARTESIAN_POINT ( 'NONE',  ( 19.99999999999999645, 24.01204443665271882, -60.22865198596099390 ) ) ;
#15197 = CARTESIAN_POINT ( 'NONE',  ( 10.32494394706616347, -4.276731815070950127, 17.08167225064743278 ) ) ;
#15198 = EDGE_LOOP ( 'NONE', ( #8172, #10853, #3548, #15377 ) ) ;
#15199 = DIRECTION ( 'NONE',  ( 0.000000000000000000, 0.000000000000000000, 1.000000000000000000 ) ) ;
#15200 = EDGE_CURVE ( 'NONE', #14722, #9681, #13688, .T. ) ;
#15201 = DIRECTION ( 'NONE',  ( -1.000000000000000000, 0.000000000000000000, 0.000000000000000000 ) ) ;
#15202 = EDGE_LOOP ( 'NONE', ( #4095, #8614, #11266, #6204 ) ) ;
#15203 = CARTESIAN_POINT ( 'NONE',  ( -16.87108763463411165, -13.40169213801852699, -74.74090047603391440 ) ) ;
#15204 = ORIENTED_EDGE ( 'NONE', *, *, #2472, .F. ) ;
#15205 = CARTESIAN_POINT ( 'NONE',  ( 12.72792206288790950, 12.72792205982780089, 12.70542500018031262 ) ) ;
#15206 = CYLINDRICAL_SURFACE ( 'NONE', #2923, 40.00000000000000000 ) ;
#15207 = FACE_OUTER_BOUND ( 'NONE', #4502, .T. ) ;
#15208 = ORIENTED_EDGE ( 'NONE', *, *, #648, .T. ) ;
#15209 = DIRECTION ( 'NONE',  ( -1.000000000000000000, 0.000000000000000000, 0.000000000000000000 ) ) ;
#15210 = VERTEX_POINT ( 'NONE', #19619 ) ;
#15211 = FACE_OUTER_BOUND ( 'NONE', #20583, .T. ) ;
#15212 = ORIENTED_EDGE ( 'NONE', *, *, #17647, .T. ) ;
#15213 = DIRECTION ( 'NONE',  ( 1.000000000000000000, -0.000000000000000000, -0.000000000000000000 ) ) ;
#15214 = ORIENTED_EDGE ( 'NONE', *, *, #11204, .T. ) ;
#15215 = DIRECTION ( 'NONE',  ( -0.000000000000000000, -0.000000000000000000, -1.000000000000000000 ) ) ;
#15216 = DIRECTION ( 'NONE',  ( 1.000000000000000000, 0.000000000000000000, 0.000000000000000000 ) ) ;
#15217 = ITEM_DEFINED_TRANSFORMATION ( 'NONE', 'NONE', #6620,  #12461 ) ;
#15218 = CARTESIAN_POINT ( 'NONE',  ( 12.54593441562640876, -8.382925371439629458, 16.62388566884154528 ) ) ;
#15219 = ORIENTED_EDGE ( 'NONE', *, *, #4934, .F. ) ;
#15220 = CARTESIAN_POINT ( 'NONE',  ( 0.000000000000000000, 27.62776854598856602, 58.65812137499012380 ) ) ;
#15221 = DIRECTION ( 'NONE',  ( 0.000000000000000000, 1.000000000000000000, -3.469446951953615175E-16 ) ) ;
#15222 = VECTOR ( 'NONE', #3037, 1000.000000000000000 ) ;
#15223 = CARTESIAN_POINT ( 'NONE',  ( 14.79893867793683349, 2.943691925285396582, -18.44732316848092779 ) ) ;
#15224 = CYLINDRICAL_SURFACE ( 'NONE', #7477, 72.00000000007199219 ) ;
#15225 = ORIENTED_EDGE ( 'NONE', *, *, #2332, .F. ) ;
#15226 = EDGE_CURVE ( 'NONE', #14918, #7434, #15096, .T. ) ;
#15227 = FACE_OUTER_BOUND ( 'NONE', #8241, .T. ) ;
#15228 = CARTESIAN_POINT ( 'NONE',  ( -2.000000000000009770, 3.464101615137749057, -5.600000000000000533 ) ) ;
#15229 = STYLED_ITEM ( 'NONE', ( #8707 ), #3565 ) ;
#15230 = ORIENTED_EDGE ( 'NONE', *, *, #8849, .F. ) ;
#15231 = CARTESIAN_POINT ( 'NONE',  ( 5.000000000000004441, 0.000000000000000000, 0.000000000000000000 ) ) ;
#15232 = ORIENTED_EDGE ( 'NONE', *, *, #4302, .T. ) ;
#15233 = CARTESIAN_POINT ( 'NONE',  ( 7.500000000000000000, 9.184850993605147944E-16, 126.0000000000000000 ) ) ;
#15234 = CARTESIAN_POINT ( 'NONE',  ( -16.62983158437509701, 6.888301784570728614, -1.569487499819690379 ) ) ;
#15235 = VERTEX_POINT ( 'NONE', #4902 ) ;
#15236 = ORIENTED_EDGE ( 'NONE', *, *, #6643, .T. ) ;
#15237 = CARTESIAN_POINT ( 'NONE',  ( 30.00000000000000000, -170.8299878242309546, -15.48896927112552824 ) ) ;
#15238 = CIRCLE ( 'NONE', #18283, 80.00000000000000000 ) ;
#15239 = CYLINDRICAL_SURFACE ( 'NONE', #6981, 72.00000000007199219 ) ;
#15240 = CARTESIAN_POINT ( 'NONE',  ( 19.99999999999999645, -31.17893654894190902, -57.31758819669202865 ) ) ;
#15241 = FILL_AREA_STYLE_COLOUR ( '', #3582 ) ;
#15242 = CARTESIAN_POINT ( 'NONE',  ( 18.00000000000000355, -2.163824016901520597E-09, 23.30855000018031120 ) ) ;
#15243 = CARTESIAN_POINT ( 'NONE',  ( 50.00000000000000000, 36.35083268962915781, -50.00000000000000000 ) ) ;
#15244 = CARTESIAN_POINT ( 'NONE',  ( -7.500000000179346316, -1.491842754445844355, 1.631668750180312877 ) ) ;
#15245 = VECTOR ( 'NONE', #7116, 1000.000000000000000 ) ;
#15246 = LINE ( 'NONE', #729, #2643 ) ;
#15247 = CARTESIAN_POINT ( 'NONE',  ( 7.902369978624323110, 7.902369976724394895, -10.65823475028680356 ) ) ;
#15248 = LINE ( 'NONE', #10709, #17519 ) ;
#15249 = ORIENTED_EDGE ( 'NONE', *, *, #13003, .T. ) ;
#15250 = ADVANCED_BREP_SHAPE_REPRESENTATION ( '', ( #3497, #12461 ), #2587 ) ;
#15251 = ADVANCED_FACE ( 'NONE', ( #18040 ), #11372, .T. ) ;
#15252 = CARTESIAN_POINT ( 'NONE',  ( 0.000000000000000000, 23.08379033237438094, -61.02926039941409897 ) ) ;
#15253 = AXIS2_PLACEMENT_3D ( 'NONE', #15100, #19758, #19957 ) ;
#15254 = CARTESIAN_POINT ( 'NONE',  ( 15.25966317163202746, 10.19618095047498407, -5.850043749819688443 ) ) ;
#15255 = CARTESIAN_POINT ( 'NONE',  ( -21.50000000000000000, 2.632990618166809235E-15, 68.00000000000000000 ) ) ;
#15256 = ORIENTED_EDGE ( 'NONE', *, *, #2731, .T. ) ;
#15257 = CARTESIAN_POINT ( 'NONE',  ( 30.00000000000000000, -39.99999999999999289, -54.09999999999998721 ) ) ;
#15258 = ORIENTED_EDGE ( 'NONE', *, *, #10209, .T. ) ;
#15259 = DIRECTION ( 'NONE',  ( -1.000000000000000000, 0.000000000000000000, -0.000000000000000000 ) ) ;
#15260 = CARTESIAN_POINT ( 'NONE',  ( 19.99999999999999645, 0.000000000000000000, 0.000000000000000000 ) ) ;
#15261 = EDGE_LOOP ( 'NONE', ( #118, #10458 ) ) ;
#15262 = AXIS2_PLACEMENT_3D ( 'NONE', #5500, #12186, #15374 ) ;
#15263 = ORIENTED_EDGE ( 'NONE', *, *, #20300, .F. ) ;
#15264 = DIRECTION ( 'NONE',  ( 1.000000000000000000, 0.000000000000000000, 0.000000000000000000 ) ) ;
#15265 = EDGE_CURVE ( 'NONE', #13795, #8524, #14963, .T. ) ;
#15266 = FILL_AREA_STYLE ('',( #4357 ) ) ;
#15267 = LINE ( 'NONE', #2442, #4853 ) ;
#15268 = DIRECTION ( 'NONE',  ( 1.000000000000000000, 0.000000000000000000, 0.000000000000000000 ) ) ;
#15269 = CARTESIAN_POINT ( 'NONE',  ( 1.491842754445842134, -7.500000000179339210, 2.435518750180311276 ) ) ;
#15270 = DIRECTION ( 'NONE',  ( -1.000000000000000000, -0.000000000000000000, -0.000000000000000000 ) ) ;
#15271 = DIRECTION ( 'NONE',  ( 0.000000000000000000, 0.000000000000000000, -1.000000000000000000 ) ) ;
#15272 = FACE_OUTER_BOUND ( 'NONE', #15079, .T. ) ;
#15273 = CARTESIAN_POINT ( 'NONE',  ( -30.00000000000000000, -124.9999999999999858, -90.00000000000001421 ) ) ;
#15274 = ORIENTED_EDGE ( 'NONE', *, *, #10528, .F. ) ;
#15275 = CARTESIAN_POINT ( 'NONE',  ( 52.00000000000000000, -39.99999999999999289, 0.000000000000000000 ) ) ;
#15276 = ORIENTED_EDGE ( 'NONE', *, *, #12963, .T. ) ;
#15277 = CARTESIAN_POINT ( 'NONE',  ( -15.25966317163203279, -10.19618095047498052, 6.382856250180313218 ) ) ;
#15278 = CARTESIAN_POINT ( 'NONE',  ( -13.88581415360056326, -16.42997871820714906, 72.99065141121243983 ) ) ;
#15279 = CIRCLE ( 'NONE', #2075, 27.60000000002760245 ) ;
#15280 = ORIENTED_EDGE ( 'NONE', *, *, #10892, .F. ) ;
#15281 = CYLINDRICAL_SURFACE ( 'NONE', #4170, 27.60000000002760245 ) ;
#15282 = ORIENTED_EDGE ( 'NONE', *, *, #19581, .T. ) ;
#15283 = CYLINDRICAL_SURFACE ( 'NONE', #4435, 27.60000000002760245 ) ;
#15284 = DIRECTION ( 'NONE',  ( -1.000000000000000000, -0.000000000000000000, -0.000000000000000000 ) ) ;
#15285 = EDGE_LOOP ( 'NONE', ( #12375, #12136 ) ) ;
#15286 = DIRECTION ( 'NONE',  ( -1.000000000000000000, 0.000000000000000000, 0.000000000000000000 ) ) ;
#15287 = AXIS2_PLACEMENT_3D ( 'NONE', #9588, #2811, #6403 ) ;
#15288 = EDGE_CURVE ( 'NONE', #11798, #10778, #5010, .T. ) ;
#15289 = AXIS2_PLACEMENT_3D ( 'NONE', #7327, #7755, #20256 ) ;
#15290 = ADVANCED_FACE ( 'NONE', ( #235 ), #1727, .T. ) ;
#15291 = VECTOR ( 'NONE', #16832, 1000.000000000000000 ) ;
#15292 = CARTESIAN_POINT ( 'NONE',  ( 7.500000000000004441, -8.788009017158368372E-15, -9.051199999997692203 ) ) ;
#15293 = CARTESIAN_POINT ( 'NONE',  ( -17.99999999999999645, 2.163826221265758470E-09, -2.158549999819691312 ) ) ;
#15294 = CYLINDRICAL_SURFACE ( 'NONE', #8947, 17.50000000000000355 ) ;
#15295 = CARTESIAN_POINT ( 'NONE',  ( -24.99999999999999289, -29.99999999999999289, -58.09475019311125976 ) ) ;
#15296 = EDGE_CURVE ( 'NONE', #8436, #18021, #9975, .T. ) ;
#15297 = CARTESIAN_POINT ( 'NONE',  ( -6.330490856366295382, 9.474249098604511587, -5.597233999352570599 ) ) ;
#15298 = PRODUCT_RELATED_PRODUCT_CATEGORY ( 'part', '', ( #18644 ) ) ;
#15299 = ORIENTED_EDGE ( 'NONE', *, *, #6830, .T. ) ;
#15300 = DIRECTION ( 'NONE',  ( -1.000000000000000000, -0.000000000000000000, -0.000000000000000000 ) ) ;
#15301 = DIRECTION ( 'NONE',  ( -1.000000000000000000, 0.000000000000000000, 0.000000000000000000 ) ) ;
#15302 = ORIENTED_EDGE ( 'NONE', *, *, #12206, .F. ) ;
#15303 = AXIS2_PLACEMENT_3D ( 'NONE', #5175, #11646, #3585 ) ;
#15304 = CARTESIAN_POINT ( 'NONE',  ( -10.58466049171558865, -18.71773173394921486, -71.82544846116152826 ) ) ;
#15305 = CIRCLE ( 'NONE', #9891, 72.00000000007199219 ) ;
#15306 = VERTEX_POINT ( 'NONE', #8179 ) ;
#15307 = CARTESIAN_POINT ( 'NONE',  ( 12.72792206288790950, 12.72792205982780089, 3.280425000180314132 ) ) ;
#15308 = AXIS2_PLACEMENT_3D ( 'NONE', #1600, #17910, #13031 ) ;
#15309 = FACE_OUTER_BOUND ( 'NONE', #9688, .T. ) ;
#15310 = DIRECTION ( 'NONE',  ( 0.000000000000000000, 0.000000000000000000, 1.000000000000000000 ) ) ;
#15311 = ORIENTED_EDGE ( 'NONE', *, *, #9224, .T. ) ;
#15312 = EDGE_CURVE ( 'NONE', #2829, #18621, #1928, .T. ) ;
#15313 = CARTESIAN_POINT ( 'NONE',  ( 19.99999999999999645, 53.26727847779603309, -48.44168704307575979 ) ) ;
#15314 = VERTEX_POINT ( 'NONE', #14860 ) ;
#15315 = CARTESIAN_POINT ( 'NONE',  ( -2.000000000000009770, 3.464101615137749057, -5.600000000000000533 ) ) ;
#15316 = CIRCLE ( 'NONE', #9569, 27.60000000002759535 ) ;
#15317 = B_SPLINE_CURVE_WITH_KNOTS ( 'NONE', 3,
 ( #926, #7372, #2820, #17135, #13849, #20294 ),
 .UNSPECIFIED., .F., .F.,
 ( 4, 2, 4 ),
 ( 0.004120275011746843581, 0.005288420935197119671, 0.006456566858647394894 ),
 .UNSPECIFIED. ) ;
#15318 = ORIENTED_EDGE ( 'NONE', *, *, #18694, .T. ) ;
#15319 = FACE_OUTER_BOUND ( 'NONE', #14953, .T. ) ;
#15320 = EDGE_CURVE ( 'NONE', #5544, #19012, #3612, .T. ) ;
#15321 = EDGE_CURVE ( 'NONE', #10201, #8657, #496, .T. ) ;
#15322 = LINE ( 'NONE', #19774, #4309 ) ;
#15323 = EDGE_CURVE ( 'NONE', #8227, #18180, #10656, .T. ) ;
#15324 = AXIS2_PLACEMENT_3D ( 'NONE', #1, #12941, #9757 ) ;
#15325 = CARTESIAN_POINT ( 'NONE',  ( -25.39999999999999858, 0.000000000000000000, 0.000000000000000000 ) ) ;
#15326 = CONTEXT_DEPENDENT_SHAPE_REPRESENTATION ( #19675, #15428 ) ;
#15327 = CARTESIAN_POINT ( 'NONE',  ( 5.663308650141532397, 13.67243654642775574, 23.39810441884155168 ) ) ;
#15328 = ORIENTED_EDGE ( 'NONE', *, *, #5239, .T. ) ;
#15329 = CARTESIAN_POINT ( 'NONE',  ( 19.99999999999999645, 60.40676135667438729, 23.56039007469059143 ) ) ;
#15330 = ORIENTED_EDGE ( 'NONE', *, *, #16553, .F. ) ;
#15331 = CARTESIAN_POINT ( 'NONE',  ( 6.177131623262577698, 0.000000000000000000, 0.000000000000000000 ) ) ;
#15332 = CARTESIAN_POINT ( 'NONE',  ( -15.25966317163202923, -10.19618095047497874, 15.80785625018031304 ) ) ;
#15333 = CARTESIAN_POINT ( 'NONE',  ( 0.000000000000000000, -15.58726123847806200, -62.93731870009420959 ) ) ;
#15334 = AXIS2_PLACEMENT_3D ( 'NONE', #12685, #20615, #14065 ) ;
#15335 = CIRCLE ( 'NONE', #1807, 27.60000000002759890 ) ;
#15336 = EDGE_CURVE ( 'NONE', #2494, #8092, #17885, .T. ) ;
#15337 = VERTEX_POINT ( 'NONE', #9679 ) ;
#15338 = FACE_OUTER_BOUND ( 'NONE', #6728, .T. ) ;
#15339 = CARTESIAN_POINT ( 'NONE',  ( -0.6543461111163939581, -4.241015250120822699, -5.460849780464846148 ) ) ;
#15340 = VERTEX_POINT ( 'NONE', #8908 ) ;
#15341 = DIRECTION ( 'NONE',  ( 0.000000000000000000, 0.000000000000000000, 1.000000000000000000 ) ) ;
#15342 = ORIENTED_EDGE ( 'NONE', *, *, #6225, .T. ) ;
#15343 = CYLINDRICAL_SURFACE ( 'NONE', #5118, 27.60000000002759890 ) ;
#15344 = CARTESIAN_POINT ( 'NONE',  ( -6.888301784570736608, -16.62983158437509346, 5.499262500180311264 ) ) ;
#15345 = ORIENTED_EDGE ( 'NONE', *, *, #10958, .F. ) ;
#15346 = AXIS2_PLACEMENT_3D ( 'NONE', #1604, #199, #13144 ) ;
#15347 = ORIENTED_EDGE ( 'NONE', *, *, #6526, .T. ) ;
#15348 = CARTESIAN_POINT ( 'NONE',  ( 19.99999999999999645, -60.40676135667455071, 23.56039007469017221 ) ) ;
#15349 = VECTOR ( 'NONE', #18119, 1000.000000000000000 ) ;
#15350 = CARTESIAN_POINT ( 'NONE',  ( -15.14999999999999325, 3.245314017740474129E-16, 46.00000000000000711 ) ) ;
#15351 = DIRECTION ( 'NONE',  ( 0.000000000000000000, 0.3984010898462361783, 0.9172113015054552676 ) ) ;
#15352 = SURFACE_STYLE_FILL_AREA ( #5483 ) ;
#15353 = CARTESIAN_POINT ( 'NONE',  ( -18.00000000000000355, 2.163826221265759298E-09, 18.59605000018030907 ) ) ;
#15354 = AXIS2_PLACEMENT_3D ( 'NONE', #19313, #11472, #19526 ) ;
#15355 = CIRCLE ( 'NONE', #476, 35.00000000000000000 ) ;
#15356 = UNCERTAINTY_MEASURE_WITH_UNIT (LENGTH_MEASURE( 1.000000000000000082E-05 ), #3896, 'distance_accuracy_value', 'NONE');
#15357 = ADVANCED_FACE ( 'NONE', ( #7000 ), #5618, .T. ) ;
#15358 = CARTESIAN_POINT ( 'NONE',  ( 19.99999999999999645, -64.36139404985942747, -32.27399814043940296 ) ) ;
#15359 = CARTESIAN_POINT ( 'NONE',  ( 1.491842754445843688, -7.500000000179346316, 8.700418750180315186 ) ) ;
#15360 = DIRECTION ( 'NONE',  ( -1.000000000000000000, -0.000000000000000000, -0.000000000000000000 ) ) ;
#15361 = CARTESIAN_POINT ( 'NONE',  ( -11.17563879758427525, -2.222972768810838051, -23.91214100028680889 ) ) ;
#15362 = AXIS2_PLACEMENT_3D ( 'NONE', #4032, #8801, #5412 ) ;
#15363 = DIRECTION ( 'NONE',  ( -1.000000000000000000, 0.000000000000000000, 0.000000000000000000 ) ) ;
#15364 = CIRCLE ( 'NONE', #17404, 2.649999999999993694 ) ;
#15365 = ORIENTED_EDGE ( 'NONE', *, *, #14376, .T. ) ;
#15366 = LINE ( 'NONE', #5815, #13970 ) ;
#15367 = CARTESIAN_POINT ( 'NONE',  ( 3.580422610670020322, -18.00000000043041126, -12.32973124981968560 ) ) ;
#15368 = CARTESIAN_POINT ( 'NONE',  ( -6.679999999999999716, 11.17999999999999972, 0.000000000000000000 ) ) ;
#15369 = VECTOR ( 'NONE', #12194, 1000.000000000000000 ) ;
#15370 = ORIENTED_EDGE ( 'NONE', *, *, #7638, .T. ) ;
#15371 = DIRECTION ( 'NONE',  ( 0.000000000000000000, 0.000000000000000000, 1.000000000000000000 ) ) ;
#15372 = ORIENTED_EDGE ( 'NONE', *, *, #1243, .F. ) ;
#15373 = AXIS2_PLACEMENT_3D ( 'NONE', #4916, #6399, #9691 ) ;
#15374 = DIRECTION ( 'NONE',  ( 0.000000000000000000, -0.5195839500354404450, 0.8544194045464843512 ) ) ;
#15375 = FACE_BOUND ( 'NONE', #11795, .T. ) ;
#15376 = ORIENTED_EDGE ( 'NONE', *, *, #17670, .F. ) ;
#15377 = ORIENTED_EDGE ( 'NONE', *, *, #7095, .F. ) ;
#15378 = LINE ( 'NONE', #16865, #1585 ) ;
#15379 = CARTESIAN_POINT ( 'NONE',  ( 21.50000000000000000, 0.000000000000000000, 68.00000000000000000 ) ) ;
#15380 = EDGE_CURVE ( 'NONE', #14705, #4487, #11955, .T. ) ;
#15381 = CARTESIAN_POINT ( 'NONE',  ( 19.99999999999999645, 60.35829202194874910, 24.78524934717571426 ) ) ;
#15382 = CIRCLE ( 'NONE', #3861, 2.099999999999990763 ) ;
#15383 = CARTESIAN_POINT ( 'NONE',  ( 5.303300858261582817, -5.303300859536631329, -7.873074999819689168 ) ) ;
#15384 = DIRECTION ( 'NONE',  ( 0.000000000000000000, 0.000000000000000000, 1.000000000000000000 ) ) ;
#15385 = LINE ( 'NONE', #9428, #4418 ) ;
#15386 = CARTESIAN_POINT ( 'NONE',  ( 19.74873734152915716, 24.74873734152916072, -120.0000000000000142 ) ) ;
#15387 = CARTESIAN_POINT ( 'NONE',  ( 19.99999999999999645, 0.000000000000000000, 0.000000000000000000 ) ) ;
#15388 = ORIENTED_EDGE ( 'NONE', *, *, #2440, .F. ) ;
#15389 = CYLINDRICAL_SURFACE ( 'NONE', #14293, 8.500000000000000000 ) ;
#15390 = VERTEX_POINT ( 'NONE', #10298 ) ;
#15391 = CARTESIAN_POINT ( 'NONE',  ( 10.19618095414378800, 15.25966316918061416, 10.50629375018031375 ) ) ;
#15392 = CARTESIAN_POINT ( 'NONE',  ( 7.417002224176399316, -20.23665979631133638, 71.11836349014902225 ) ) ;
#15393 = AXIS2_PLACEMENT_3D ( 'NONE', #2955, #20740, #20544 ) ;
#15394 = VERTEX_POINT ( 'NONE', #17078 ) ;
#15395 = CARTESIAN_POINT ( 'NONE',  ( 19.99999999999999645, 0.000000000000000000, 0.000000000000000000 ) ) ;
#15396 = ORIENTED_EDGE ( 'NONE', *, *, #673, .T. ) ;
#15397 = VECTOR ( 'NONE', #8161, 1000.000000000000000 ) ;
#15398 = DIRECTION ( 'NONE',  ( -1.000000000000000000, 0.000000000000000000, 0.000000000000000000 ) ) ;
#15399 = DIRECTION ( 'NONE',  ( 0.000000000000000000, -0.000000000000000000, 1.000000000000000000 ) ) ;
#15400 = DIRECTION ( 'NONE',  ( -1.000000000000000000, 0.000000000000000000, 0.000000000000000000 ) ) ;
#15401 = ORIENTED_EDGE ( 'NONE', *, *, #2090, .T. ) ;
#15402 = DIRECTION ( 'NONE',  ( -0.000000000000000000, -1.000000000000000000, -0.000000000000000000 ) ) ;
#15403 = AXIS2_PLACEMENT_3D ( 'NONE', #6310, #10590, #8997 ) ;
#15404 = FACE_OUTER_BOUND ( 'NONE', #5142, .T. ) ;
#15405 = CARTESIAN_POINT ( 'NONE',  ( -18.00000000043040771, -3.580422610670021211, -2.453081249819692111 ) ) ;
#15406 = FACE_OUTER_BOUND ( 'NONE', #2500, .T. ) ;
#15407 = CARTESIAN_POINT ( 'NONE',  ( -8.999999999999987566, -85.00000000000000000, 5.000000000000000000 ) ) ;
#15408 = CARTESIAN_POINT ( 'NONE',  ( 10.32494394706616347, -4.276731815070950127, -1.768327749352573308 ) ) ;
#15409 = ORIENTED_EDGE ( 'NONE', *, *, #1646, .T. ) ;
#15410 = CARTESIAN_POINT ( 'NONE',  ( 50.00000000000000000, 36.35083268962917202, 90.00000000000000000 ) ) ;
#15411 = DIRECTION ( 'NONE',  ( -0.000000000000000000, -0.000000000000000000, 1.000000000000000000 ) ) ;
#15412 = ORIENTED_EDGE ( 'NONE', *, *, #3404, .T. ) ;
#15413 = DIRECTION ( 'NONE',  ( -1.000000000000000000, 5.334274688628681815E-15, 0.000000000000000000 ) ) ;
#15414 = EDGE_CURVE ( 'NONE', #9241, #19897, #13801, .T. ) ;
#15415 = VERTEX_POINT ( 'NONE', #13483 ) ;
#15416 = EDGE_CURVE ( 'NONE', #7037, #3825, #18661, .T. ) ;
#15417 = CARTESIAN_POINT ( 'NONE',  ( 16.62983158437509346, -6.888301784570739272, -4.377387499819689332 ) ) ;
#15418 = CARTESIAN_POINT ( 'NONE',  ( 30.00000000000000711, 29.99999999999998579, -130.0000000000000000 ) ) ;
#15419 = LINE ( 'NONE', #7246, #12073 ) ;
#15420 = VERTEX_POINT ( 'NONE', #20249 ) ;
#15421 = CARTESIAN_POINT ( 'NONE',  ( 19.99999999999999645, 5.762283366692075859, -64.99406197038663890 ) ) ;
#15422 = EDGE_LOOP ( 'NONE', ( #7464, #7193 ) ) ;
#15423 = CARTESIAN_POINT ( 'NONE',  ( 28.13963350654227824, -26.35784117651622793, -120.0000000000000142 ) ) ;
#15424 = ADVANCED_FACE ( 'NONE', ( #12100 ), #647, .T. ) ;
#15425 = ORIENTED_EDGE ( 'NONE', *, *, #11479, .F. ) ;
#15426 = CIRCLE ( 'NONE', #3245, 65.24900000006526568 ) ;
#15427 = DIRECTION ( 'NONE',  ( -0.000000000000000000, -0.000000000000000000, 1.000000000000000000 ) ) ;
#15428 = PRODUCT_DEFINITION_SHAPE ( 'NONE', 'NONE',  #20950 ) ;
#15429 = DIRECTION ( 'NONE',  ( -0.000000000000000000, -0.000000000000000000, 1.000000000000000000 ) ) ;
#15430 = ITEM_DEFINED_TRANSFORMATION ( 'NONE', 'NONE', #20161,  #12461 ) ;
#15431 = CARTESIAN_POINT ( 'NONE',  ( 10.46442989454075700, 10.46442989202484419, 5.137166918841548302 ) ) ;
#15432 = ADVANCED_FACE ( 'NONE', ( #11988 ), #3812, .T. ) ;
#15433 = VERTEX_POINT ( 'NONE', #18567 ) ;
#15434 = LINE ( 'NONE', #7704, #9624 ) ;
#15435 = ORIENTED_EDGE ( 'NONE', *, *, #12765, .F. ) ;
#15436 = DIRECTION ( 'NONE',  ( -1.000000000000000000, 0.000000000000000000, 0.000000000000000000 ) ) ;
#15437 = ADVANCED_FACE ( 'NONE', ( #7098 ), #751, .F. ) ;
#15438 = CARTESIAN_POINT ( 'NONE',  ( -16.62983158603121936, -6.888301780572499311, 6.677387500180310020 ) ) ;
#15439 = EDGE_CURVE ( 'NONE', #11338, #12564, #16867, .T. ) ;
#15440 = CARTESIAN_POINT ( 'NONE',  ( 50.00000000000000000, 36.35083268962915781, 50.00000000000000000 ) ) ;
#15441 = AXIS2_PLACEMENT_3D ( 'NONE', #12234, #13519, #18709 ) ;
#15442 = VECTOR ( 'NONE', #6772, 1000.000000000000000 ) ;
#15443 = ORIENTED_EDGE ( 'NONE', *, *, #5097, .T. ) ;
#15444 = AXIS2_PLACEMENT_3D ( 'NONE', #5839, #17611, #9342 ) ;
#15445 = EDGE_CURVE ( 'NONE', #19491, #1793, #2139, .T. ) ;
#15446 = DIRECTION ( 'NONE',  ( -1.000000000000000000, 0.000000000000000000, -0.000000000000000000 ) ) ;
#15447 = FACE_BOUND ( 'NONE', #13973, .T. ) ;
#15448 = ORIENTED_EDGE ( 'NONE', *, *, #11504, .F. ) ;
#15449 = DIRECTION ( 'NONE',  ( 0.000000000000000000, -3.469446951953615175E-16, -1.000000000000000000 ) ) ;
#15450 = VERTEX_POINT ( 'NONE', #16648 ) ;
#15451 = CARTESIAN_POINT ( 'NONE',  ( 0.000000000000000000, 59.31169354540775629, -27.19476070466793871 ) ) ;
#15452 = CARTESIAN_POINT ( 'NONE',  ( 16.62983158603121936, 6.888301780572501976, -16.88511249981969442 ) ) ;
#15453 = CIRCLE ( 'NONE', #16144, 65.24900000006526568 ) ;
#15454 = VERTEX_POINT ( 'NONE', #10618 ) ;
#15455 = EDGE_LOOP ( 'NONE', ( #19720, #6309, #9792, #2020 ) ) ;
#15456 = CARTESIAN_POINT ( 'NONE',  ( 30.00000000000000000, -164.9999999999999716, -50.00000000000002842 ) ) ;
#15457 = AXIS2_PLACEMENT_3D ( 'NONE', #20158, #14145, #10844 ) ;
#15458 = FACE_OUTER_BOUND ( 'NONE', #11273, .T. ) ;
#15459 = VECTOR ( 'NONE', #2868, 1000.000000000000000 ) ;
#15460 = CARTESIAN_POINT ( 'NONE',  ( 7.500000000000009770, -8.788009017158368372E-15, -2.786299999997682519 ) ) ;
#15461 = CARTESIAN_POINT ( 'NONE',  ( 0.000000000000000000, 0.000000000000000000, 0.000000000000000000 ) ) ;
#15462 =( NAMED_UNIT ( * ) PLANE_ANGLE_UNIT ( ) SI_UNIT ( $, .RADIAN. ) );
#15463 = EDGE_CURVE ( 'NONE', #10607, #15704, #8595, .T. ) ;
#15464 = CARTESIAN_POINT ( 'NONE',  ( -12.72792206288791483, -12.72792205982780089, 7.992925000180310491 ) ) ;
#15465 = EDGE_CURVE ( 'NONE', #1870, #5904, #15267, .T. ) ;
#15466 = DIRECTION ( 'NONE',  ( -1.000000000000000000, 0.000000000000000000, 0.000000000000000000 ) ) ;
#15467 = CARTESIAN_POINT ( 'NONE',  ( 6.929096494179683319, 2.870125741905213079, -3.375362499819685613 ) ) ;
#15468 = EDGE_LOOP ( 'NONE', ( #4182, #4591, #15540, #7261 ) ) ;
#15469 = LINE ( 'NONE', #5808, #11425 ) ;
#15470 = CARTESIAN_POINT ( 'NONE',  ( -4.276731815070945686, -10.32494394706615637, -15.95979725028680996 ) ) ;
#15471 = ADVANCED_FACE ( 'NONE', ( #4128 ), #2560, .F. ) ;
#15472 = AXIS2_PLACEMENT_3D ( 'NONE', #4347, #10814, #17596 ) ;
#15473 = LINE ( 'NONE', #7504, #1623 ) ;
#15474 = ORIENTED_EDGE ( 'NONE', *, *, #19033, .T. ) ;
#15475 = CARTESIAN_POINT ( 'NONE',  ( 7.500000000000000000, 9.184850993605147944E-16, 40.00000000000000000 ) ) ;
#15476 = CARTESIAN_POINT ( 'NONE',  ( -18.00000000043041126, -3.580422610670022543, -9.973481249819688088 ) ) ;
#15477 = DIRECTION ( 'NONE',  ( 1.000000000000000000, 0.000000000000000000, 0.000000000000000000 ) ) ;
#15478 = ORIENTED_EDGE ( 'NONE', *, *, #6886, .F. ) ;
#15479 = CARTESIAN_POINT ( 'NONE',  ( 0.000000000000000000, 0.000000000000000000, 0.000000000000000000 ) ) ;
#15480 = CIRCLE ( 'NONE', #8360, 2.649999999999999467 ) ;
#15481 = ORIENTED_EDGE ( 'NONE', *, *, #12542, .T. ) ;
#15482 = CARTESIAN_POINT ( 'NONE',  ( 8.900000000000041211, 10.82531754730546147, 46.00000000000000711 ) ) ;
#15483 = LINE ( 'NONE', #16861, #8333 ) ;
#15484 = ORIENTED_EDGE ( 'NONE', *, *, #16216, .T. ) ;
#15485 = EDGE_LOOP ( 'NONE', ( #18238, #5320, #12834, #4978 ) ) ;
#15486 = CARTESIAN_POINT ( 'NONE',  ( -31.74999999999995737, 5.204748896376250699E-16, -4.250000000000000000 ) ) ;
#15487 = PLANE ( 'NONE',  #12296 ) ;
#15488 = AXIS2_PLACEMENT_3D ( 'NONE', #9487, #19443, #1852 ) ;
#15489 = CARTESIAN_POINT ( 'NONE',  ( 62.50000000000000000, -120.0000000000000142, 5.000000000000000000 ) ) ;
#15490 = CARTESIAN_POINT ( 'NONE',  ( -6.929096493489625530, 2.870125743571138255, -3.749637499819689079 ) ) ;
#15491 = CARTESIAN_POINT ( 'NONE',  ( 19.99999999999999645, 42.42902769288536291, 49.02903636734212967 ) ) ;
#15492 = DIRECTION ( 'NONE',  ( -1.000000000000000000, -0.000000000000000000, 0.000000000000000000 ) ) ;
#15493 = DIRECTION ( 'NONE',  ( 0.000000000000000000, -0.9790840876823205807, -0.2034560130526446575 ) ) ;
#15494 = CARTESIAN_POINT ( 'NONE',  ( 9.999999999999998224, -58.26603306961936113, -42.29739224042532442 ) ) ;
#15495 = EDGE_LOOP ( 'NONE', ( #16704, #4695, #9529 ) ) ;
#15496 = CARTESIAN_POINT ( 'NONE',  ( -10.00000000000000000, 0.000000000000000000, 0.000000000000000000 ) ) ;
#15497 = ORIENTED_EDGE ( 'NONE', *, *, #7995, .T. ) ;
#15498 = CARTESIAN_POINT ( 'NONE',  ( 18.00000000000000000, -2.163824016901520184E-09, 11.97895000018031375 ) ) ;
#15499 = DIRECTION ( 'NONE',  ( -1.000000000000000000, -0.000000000000000000, -0.000000000000000000 ) ) ;
#15500 = VERTEX_POINT ( 'NONE', #2136 ) ;
#15501 = DIRECTION ( 'NONE',  ( 0.000000000000000000, -0.000000000000000000, 1.000000000000000000 ) ) ;
#15502 = ORIENTED_EDGE ( 'NONE', *, *, #12715, .T. ) ;
#15503 = LINE ( 'NONE', #10523, #15245 ) ;
#15504 = DIRECTION ( 'NONE',  ( 0.000000000000000000, 1.224646799147353207E-16, 1.000000000000000000 ) ) ;
#15505 = CARTESIAN_POINT ( 'NONE',  ( 19.99999999999999645, 0.000000000000000000, 0.000000000000000000 ) ) ;
#15506 = ADVANCED_FACE ( 'NONE', ( #2342, #9024 ), #15487, .T. ) ;
#15507 = ORIENTED_EDGE ( 'NONE', *, *, #16603, .F. ) ;
#15508 = DIRECTION ( 'NONE',  ( 0.000000000000000000, 0.9790840876823220240, 0.2034560130526376631 ) ) ;
#15509 = CARTESIAN_POINT ( 'NONE',  ( 45.22159793441011999, -8.673994507468384185, 84.62946326583127643 ) ) ;
#15510 = DIRECTION ( 'NONE',  ( 0.000000000000000000, 0.000000000000000000, -1.000000000000000000 ) ) ;
#15511 = DIRECTION ( 'NONE',  ( 0.000000000000000000, 0.000000000000000000, 1.000000000000000000 ) ) ;
#15512 = CYLINDRICAL_SURFACE ( 'NONE', #6557, 65.24900000006525147 ) ;
#15513 = ORIENTED_EDGE ( 'NONE', *, *, #14264, .T. ) ;
#15514 = DIRECTION ( 'NONE',  ( -0.000000000000000000, -0.000000000000000000, 1.000000000000000000 ) ) ;
#15515 = VERTEX_POINT ( 'NONE', #20134 ) ;
#15516 = CARTESIAN_POINT ( 'NONE',  ( 5.982253535725074123, -20.70709046307243995, -70.91533586927070587 ) ) ;
#15517 = DIRECTION ( 'NONE',  ( -1.000000000000000000, 0.000000000000000000, 0.000000000000000000 ) ) ;
#15518 = EDGE_LOOP ( 'NONE', ( #20178, #12751, #19650, #6785 ) ) ;
#15519 = CARTESIAN_POINT ( 'NONE',  ( 18.00000000000000000, -2.163824016901520184E-09, -4.966449999819686489 ) ) ;
#15520 = CARTESIAN_POINT ( 'NONE',  ( 93.70999227554992217, -50.00000000000000000, -90.00000000000001421 ) ) ;
#15521 = CARTESIAN_POINT ( 'NONE',  ( 19.99999999999999645, 60.35829202194874910, 24.78524934717571426 ) ) ;
#15522 = ORIENTED_EDGE ( 'NONE', *, *, #8425, .F. ) ;
#15523 = CARTESIAN_POINT ( 'NONE',  ( -25.00000000000000000, -30.00000000000000711, 58.09475019311124555 ) ) ;
#15524 = VERTEX_POINT ( 'NONE', #13577 ) ;
#15525 = DIRECTION ( 'NONE',  ( 0.000000000000000000, 0.5000000000000011102, 0.8660254037844380415 ) ) ;
#15526 = ADVANCED_FACE ( 'NONE', ( #20024 ), #15900, .T. ) ;
#15527 = ORIENTED_EDGE ( 'NONE', *, *, #8702, .F. ) ;
#15528 = CARTESIAN_POINT ( 'NONE',  ( 4.000000000000003553, -0.3902508023145557225, -5.599999999999998757 ) ) ;
#15529 = ADVANCED_FACE ( 'NONE', ( #10823 ), #14326, .T. ) ;
#15530 = DIRECTION ( 'NONE',  ( 0.000000000000000000, 0.000000000000000000, 1.000000000000000000 ) ) ;
#15531 = CARTESIAN_POINT ( 'NONE',  ( 14.79893867758297610, -1.779016607511492805E-09, 6.315291918841546170 ) ) ;
#15532 = VERTEX_POINT ( 'NONE', #20773 ) ;
#15533 = DIRECTION ( 'NONE',  ( -1.000000000000000000, -0.000000000000000000, -0.000000000000000000 ) ) ;
#15534 = ORIENTED_EDGE ( 'NONE', *, *, #4751, .F. ) ;
#15535 = EDGE_CURVE ( 'NONE', #2751, #10315, #1191, .T. ) ;
#15536 = CARTESIAN_POINT ( 'NONE',  ( 50.00000000000000000, 36.35083268962915781, 50.00000000000000000 ) ) ;
#15537 = CARTESIAN_POINT ( 'NONE',  ( 12.72792205982779379, -12.72792206288790950, 13.15707500018031162 ) ) ;
#15538 = CARTESIAN_POINT ( 'NONE',  ( 2.500000000000000000, 2.357898499370431722, -2.818925648462311528E-15 ) ) ;
#15539 = CARTESIAN_POINT ( 'NONE',  ( 19.99999999999999645, 62.46228066917787203, 18.86519267363478036 ) ) ;
#15540 = ORIENTED_EDGE ( 'NONE', *, *, #19190, .F. ) ;
#15541 = DIRECTION ( 'NONE',  ( 1.000000000000000000, 0.000000000000000000, 0.000000000000000000 ) ) ;
#15542 = CARTESIAN_POINT ( 'NONE',  ( 10.00000000000000178, -164.9999999999999716, 70.00000000000000000 ) ) ;
#15543 = ORIENTED_EDGE ( 'NONE', *, *, #11936, .F. ) ;
#15544 = LINE ( 'NONE', #10470, #20734 ) ;
#15545 = CARTESIAN_POINT ( 'NONE',  ( 19.99999999999999645, 0.000000000000000000, 0.000000000000000000 ) ) ;
#15546 = CARTESIAN_POINT ( 'NONE',  ( -16.62983158603121936, -6.888301780572499311, -12.17261249981969229 ) ) ;
#15547 = ORIENTED_EDGE ( 'NONE', *, *, #12308, .T. ) ;
#15548 = ORIENTED_EDGE ( 'NONE', *, *, #9135, .F. ) ;
#15549 = DIRECTION ( 'NONE',  ( 0.000000000000000000, 0.000000000000000000, -1.000000000000000000 ) ) ;
#15550 = EDGE_CURVE ( 'NONE', #5709, #12561, #18066, .T. ) ;
#15551 = DIRECTION ( 'NONE',  ( 0.000000000000000000, 0.000000000000000000, 1.000000000000000000 ) ) ;
#15552 = EDGE_CURVE ( 'NONE', #14202, #18745, #8911, .T. ) ;
#15553 = DIRECTION ( 'NONE',  ( 1.000000000000000000, 0.000000000000000000, 0.000000000000000000 ) ) ;
#15554 = DIRECTION ( 'NONE',  ( -1.000000000000000000, -0.000000000000000000, -0.000000000000000000 ) ) ;
#15555 =( NAMED_UNIT ( * ) PLANE_ANGLE_UNIT ( ) SI_UNIT ( $, .RADIAN. ) );
#15556 = CARTESIAN_POINT ( 'NONE',  ( -10.19618095414378800, -15.25966316918061771, -1.726606249819691463 ) ) ;
#15557 = CIRCLE ( 'NONE', #6416, 65.24900000006525147 ) ;
#15558 = UNCERTAINTY_MEASURE_WITH_UNIT (LENGTH_MEASURE( 1.000000000000000082E-05 ), #18543, 'distance_accuracy_value', 'NONE');
#15559 = ADVANCED_FACE ( 'NONE', ( #7746 ), #17606, .T. ) ;
#15560 = CARTESIAN_POINT ( 'NONE',  ( 5.303300859536635770, 5.303300858261589923, -13.38942499981969014 ) ) ;
#15561 = ADVANCED_FACE ( 'NONE', ( #9127 ), #5828, .T. ) ;
#15562 = ORIENTED_EDGE ( 'NONE', *, *, #13905, .T. ) ;
#15563 = PRODUCT_DEFINITION ( 'UNKNOWN', '', #10323, #11963 ) ;
#15564 = CARTESIAN_POINT ( 'NONE',  ( 1.491842754445843688, -7.500000000179346316, 18.12541875018031945 ) ) ;
#15565 = CARTESIAN_POINT ( 'NONE',  ( -12.54593441764187034, -8.382925368423267187, 13.95111433151907754 ) ) ;
#15566 = DIRECTION ( 'NONE',  ( 0.000000000000000000, 0.000000000000000000, -1.000000000000000000 ) ) ;
#15567 = VERTEX_POINT ( 'NONE', #19194 ) ;
#15568 = CYLINDRICAL_SURFACE ( 'NONE', #2788, 65.24900000006525147 ) ;
#15569 = CARTESIAN_POINT ( 'NONE',  ( -10.19618095047498052, 15.25966317163203101, -17.63129374981969022 ) ) ;
#15570 = DIRECTION ( 'NONE',  ( 0.000000000000000000, 0.9976687691905394839, -0.06824241336466758956 ) ) ;
#15571 = ADVANCED_FACE ( 'NONE', ( #2869, #4247 ), #11029, .T. ) ;
#15572 = ORIENTED_EDGE ( 'NONE', *, *, #2631, .F. ) ;
#15573 = EDGE_CURVE ( 'NONE', #197, #1438, #17721, .T. ) ;
#15574 = DIRECTION ( 'NONE',  ( -1.000000000000000000, -0.000000000000000000, -0.000000000000000000 ) ) ;
#15575 = ORIENTED_EDGE ( 'NONE', *, *, #19395, .T. ) ;
#15576 = DIRECTION ( 'NONE',  ( 0.000000000000000000, 0.9976687691905389288, 0.06824241336467461172 ) ) ;
#15577 = CARTESIAN_POINT ( 'NONE',  ( 19.99999999999999645, -54.08351995568730786, 35.76369202524482915 ) ) ;
#15578 = VECTOR ( 'NONE', #1226, 1000.000000000000000 ) ;
#15579 = VERTEX_POINT ( 'NONE', #6046 ) ;
#15580 = ORIENTED_EDGE ( 'NONE', *, *, #3453, .T. ) ;
#15581 = CARTESIAN_POINT ( 'NONE',  ( 30.00000000000000000, -50.00000000000000000, -90.00000000000001421 ) ) ;
#15582 = EDGE_CURVE ( 'NONE', #11, #13626, #4673, .T. ) ;
#15583 = AXIS2_PLACEMENT_3D ( 'NONE', #8499, #14673, #9998 ) ;
#15584 = CARTESIAN_POINT ( 'NONE',  ( 19.99999999999999645, 0.000000000000000000, 0.000000000000000000 ) ) ;
#15585 = ADVANCED_FACE ( 'NONE', ( #15797 ), #7420, .F. ) ;
#15586 = DIRECTION ( 'NONE',  ( 0.000000000000000000, -1.000000000000000000, 0.000000000000000000 ) ) ;
#15587 = CARTESIAN_POINT ( 'NONE',  ( 7.500000000000000888, -9.015933403756337545E-10, -27.90119999981969556 ) ) ;
#15588 = AXIS2_PLACEMENT_3D ( 'NONE', #10219, #2059, #8625 ) ;
#15589 = DIRECTION ( 'NONE',  ( 1.000000000000000000, 0.000000000000000000, 0.000000000000000000 ) ) ;
#15590 = CARTESIAN_POINT ( 'NONE',  ( 54.64999999999999858, -39.99999999999999289, 5.000000000000000000 ) ) ;
#15591 = CIRCLE ( 'NONE', #1054, 4.000000000000000888 ) ;
#15592 = ORIENTED_EDGE ( 'NONE', *, *, #2892, .T. ) ;
#15593 = CARTESIAN_POINT ( 'NONE',  ( 0.000000000000000000, 0.000000000000000000, 0.000000000000000000 ) ) ;
#15594 = VERTEX_POINT ( 'NONE', #7846 ) ;
#15595 = CARTESIAN_POINT ( 'NONE',  ( -16.62983158437510056, 6.888301784570729502, -20.41948749981968803 ) ) ;
#15596 = CARTESIAN_POINT ( 'NONE',  ( 20.00000000000000355, 9.184850993605147944E-16, -7.500000000000000000 ) ) ;
#15597 = ORIENTED_EDGE ( 'NONE', *, *, #14025, .T. ) ;
#15598 = EDGE_CURVE ( 'NONE', #17111, #14031, #10726, .T. ) ;
#15599 = DIRECTION ( 'NONE',  ( -0.000000000000000000, 1.000000000000000000, 0.000000000000000000 ) ) ;
#15600 = VERTEX_POINT ( 'NONE', #14009 ) ;
#15601 = DIRECTION ( 'NONE',  ( -1.000000000000000000, -0.000000000000000000, -0.000000000000000000 ) ) ;
#15602 = DIRECTION ( 'NONE',  ( 0.000000000000000000, 0.000000000000000000, -1.000000000000000000 ) ) ;
#15603 = LINE ( 'NONE', #17531, #20175 ) ;
#15604 = ORIENTED_EDGE ( 'NONE', *, *, #15550, .T. ) ;
#15605 = DIRECTION ( 'NONE',  ( -1.000000000000000000, 0.000000000000000000, 0.000000000000000000 ) ) ;
#15606 = CARTESIAN_POINT ( 'NONE',  ( -40.00000000000000000, 29.99999999999999289, -120.0000000000000142 ) ) ;
#15607 = CARTESIAN_POINT ( 'NONE',  ( -12.72792206288790950, -12.72792205982779556, -22.18667499981969726 ) ) ;
#15608 = DIRECTION ( 'NONE',  ( -1.000000000000000000, -0.000000000000000000, -0.000000000000000000 ) ) ;
#15609 = CIRCLE ( 'NONE', #15958, 3.199999999999994404 ) ;
#15610 = DIRECTION ( 'NONE',  ( -0.000000000000000000, 1.000000000000000000, 1.224646799147353207E-16 ) ) ;
#15611 = AXIS2_PLACEMENT_3D ( 'NONE', #3203, #17935, #9864 ) ;
#15612 = ORIENTED_EDGE ( 'NONE', *, *, #15982, .T. ) ;
#15613 =( NAMED_UNIT ( * ) SI_UNIT ( $, .STERADIAN. ) SOLID_ANGLE_UNIT ( ) );
#15614 = EDGE_CURVE ( 'NONE', #16659, #11587, #15692, .T. ) ;
#15615 = LINE ( 'NONE', #14153, #9822 ) ;
#15616 = EDGE_LOOP ( 'NONE', ( #12207, #5271, #5200, #195 ) ) ;
#15617 = AXIS2_PLACEMENT_3D ( 'NONE', #17047, #12275, #12594 ) ;
#15618 = LINE ( 'NONE', #1228, #16703 ) ;
#15619 = DIRECTION ( 'NONE',  ( -0.000000000000000000, -0.000000000000000000, 1.000000000000000000 ) ) ;
#15620 = ORIENTED_EDGE ( 'NONE', *, *, #17713, .T. ) ;
#15621 = CARTESIAN_POINT ( 'NONE',  ( -10.19618095047498052, 15.25966317163203101, -17.63129374981968667 ) ) ;
#15622 = DIRECTION ( 'NONE',  ( -1.000000000000000000, -8.673617379884035472E-17, 0.000000000000000000 ) ) ;
#15623 = DIRECTION ( 'NONE',  ( 0.000000000000000000, 0.000000000000000000, 1.000000000000000000 ) ) ;
#15624 = VERTEX_POINT ( 'NONE', #7637 ) ;
#15625 = AXIS2_PLACEMENT_3D ( 'NONE', #13698, #16455, #18464 ) ;
#15626 = DIRECTION ( 'NONE',  ( 0.000000000000000000, 0.6310879443260486443, 0.7757112907044232397 ) ) ;
#15627 = VERTEX_POINT ( 'NONE', #20462 ) ;
#15628 = CARTESIAN_POINT ( 'NONE',  ( -65.00002539999999840, 0.000000000000000000, -1.000000000000000000 ) ) ;
#15629 = AXIS2_PLACEMENT_3D ( 'NONE', #6552, #6444, #13234 ) ;
#15630 = ORIENTED_EDGE ( 'NONE', *, *, #15640, .T. ) ;
#15631 =( REPRESENTATION_RELATIONSHIP ('NONE','NONE', #13739, #11016 ) REPRESENTATION_RELATIONSHIP_WITH_TRANSFORMATION ( #13634 )SHAPE_REPRESENTATION_RELATIONSHIP( ) );
#15632 = AXIS2_PLACEMENT_3D ( 'NONE', #1160, #20540, #6427 ) ;
#15633 = CARTESIAN_POINT ( 'NONE',  ( 32.34000317368597877, -114.4267062510364354, 75.39615112841575240 ) ) ;
#15634 = CYLINDRICAL_SURFACE ( 'NONE', #20418, 7.500000000000000000 ) ;
#15635 = CONTEXT_DEPENDENT_SHAPE_REPRESENTATION ( #16435, #6946 ) ;
#15636 = CARTESIAN_POINT ( 'NONE',  ( -14.79893867793684059, -2.943691925285399691, 1.308260668841543461 ) ) ;
#15637 = AXIS2_PLACEMENT_3D ( 'NONE', #11918, #10667, #802 ) ;
#15639 = ORIENTED_EDGE ( 'NONE', *, *, #2084, .F. ) ;
#15638 = AXIS2_PLACEMENT_3D ( 'NONE', #536, #427, #11550 ) ;
#15640 = EDGE_CURVE ( 'NONE', #6966, #5326, #1142, .T. ) ;
#15641 = CARTESIAN_POINT ( 'NONE',  ( 49.35000000000000142, -39.99999999999999289, 5.000000000000000000 ) ) ;
#15642 = CIRCLE ( 'NONE', #18689, 27.60000000002759890 ) ;
#15643 = ORIENTED_EDGE ( 'NONE', *, *, #12482, .T. ) ;
#15644 = CARTESIAN_POINT ( 'NONE',  ( 8.948086041649604638, -19.56205492480948038, 76.99190269118484764 ) ) ;
#15645 = CARTESIAN_POINT ( 'NONE',  ( 18.00000000043040771, 3.580422610670018546, 11.68441875018031162 ) ) ;
#15646 = CARTESIAN_POINT ( 'NONE',  ( 21.00000000000000000, 2.055000000000000160, 0.000000000000000000 ) ) ;
#15647 = LINE ( 'NONE', #7711, #4616 ) ;
#15648 = EDGE_LOOP ( 'NONE', ( #11092, #7311, #9839, #16908 ) ) ;
#15649 = DIRECTION ( 'NONE',  ( -1.000000000000000000, 0.000000000000000000, 0.000000000000000000 ) ) ;
#15650 = DIRECTION ( 'NONE',  ( 0.000000000000000000, -6.982962677686266711E-15, 1.000000000000000000 ) ) ;
#15651 = VERTEX_POINT ( 'NONE', #5941 ) ;
#15652 = AXIS2_PLACEMENT_3D ( 'NONE', #12496, #11000, #18957 ) ;
#15653 = CARTESIAN_POINT ( 'NONE',  ( 20.06332430260529520, -11.25004336140582417, -82.40911568055234682 ) ) ;
#15654 = CIRCLE ( 'NONE', #10924, 27.60000000002760245 ) ;
#15655 = DIRECTION ( 'NONE',  ( -1.000000000000000000, 0.000000000000000000, 0.000000000000000000 ) ) ;
#15656 = CARTESIAN_POINT ( 'NONE',  ( 12.72792206288790773, 12.72792205982779912, -17.47417499981969513 ) ) ;
#15657 = CIRCLE ( 'NONE', #4481, 27.60000000002759180 ) ;
#15658 = VECTOR ( 'NONE', #9094, 1000.000000000000000 ) ;
#15659 = ORIENTED_EDGE ( 'NONE', *, *, #18148, .F. ) ;
#15660 = CARTESIAN_POINT ( 'NONE',  ( -7.500000000000009770, -1.491842754878800248, -7.793331249912205827 ) ) ;
#15661 = DIRECTION ( 'NONE',  ( -1.000000000000000000, 0.000000000000000000, 0.000000000000000000 ) ) ;
#15662 = CARTESIAN_POINT ( 'NONE',  ( 8.900000000000046541, 10.82531754730546147, 46.00000000000000711 ) ) ;
#15663 = CARTESIAN_POINT ( 'NONE',  ( 30.00000000000000000, -84.99999999999998579, -75.00000000000001421 ) ) ;
#15664 = CARTESIAN_POINT ( 'NONE',  ( 6.249999999999905853, -10.82531754730554496, -39.99999999999999289 ) ) ;
#15665 = CARTESIAN_POINT ( 'NONE',  ( -15.25966316918061949, 10.19618095414378800, 0.6296437501803093806 ) ) ;
#15666 = CARTESIAN_POINT ( 'NONE',  ( -7.499999999820669672, 1.491842756249032620, -16.62926874981969050 ) ) ;
#15667 = ORIENTED_EDGE ( 'NONE', *, *, #9002, .T. ) ;
#15668 = AXIS2_PLACEMENT_3D ( 'NONE', #11926, #3868, #8750 ) ;
#15669 = DIRECTION ( 'NONE',  ( -1.000000000000000000, -0.000000000000000000, -0.000000000000000000 ) ) ;
#15670 = AXIS2_PLACEMENT_3D ( 'NONE', #3422, #16358, #16257 ) ;
#15671 = CARTESIAN_POINT ( 'NONE',  ( -5.663308646854335215, 13.67243654778934925, 16.60189558151908074 ) ) ;
#15672 = DIRECTION ( 'NONE',  ( 1.000000000000000000, 0.000000000000000000, 0.000000000000000000 ) ) ;
#15673 = EDGE_CURVE ( 'NONE', #16021, #11056, #4358, .T. ) ;
#15674 = ORIENTED_EDGE ( 'NONE', *, *, #7812, .F. ) ;
#15675 = DIRECTION ( 'NONE',  ( -1.000000000000000000, -0.000000000000000000, -0.000000000000000000 ) ) ;
#15676 = ADVANCED_FACE ( 'NONE', ( #14535 ), #7960, .T. ) ;
#15677 = CARTESIAN_POINT ( 'NONE',  ( 19.99999999999999645, -65.23577793412343340, -1.313498510942392450 ) ) ;
#15678 = CARTESIAN_POINT ( 'NONE',  ( 9.999999999999998224, 68.15657073222466522, -23.20952102120210725 ) ) ;
#15679 = AXIS2_PLACEMENT_3D ( 'NONE', #9837, #8058, #16306 ) ;
#15680 = ORIENTED_EDGE ( 'NONE', *, *, #1103, .F. ) ;
#15681 = AXIS2_PLACEMENT_3D ( 'NONE', #16757, #11780, #15069 ) ;
#15682 = CARTESIAN_POINT ( 'NONE',  ( 0.000000000000000000, 0.000000000000000000, -81.99999999999998579 ) ) ;
#15683 = ORIENTED_EDGE ( 'NONE', *, *, #15037, .T. ) ;
#15684 = CARTESIAN_POINT ( 'NONE',  ( 30.43430782549247837, -42.57363661491096707, -71.38288848018790134 ) ) ;
#15685 = CYLINDRICAL_SURFACE ( 'NONE', #20191, 27.60000000002759890 ) ;
#15686 = ORIENTED_EDGE ( 'NONE', *, *, #6244, .F. ) ;
#15687 = EDGE_CURVE ( 'NONE', #4041, #19846, #10952, .T. ) ;
#15688 = VERTEX_POINT ( 'NONE', #19599 ) ;
#15689 = CARTESIAN_POINT ( 'NONE',  ( 2.500000000000000000, -2.357898499370432166, 3.035766082959412415E-15 ) ) ;
#15690 = AXIS2_PLACEMENT_3D ( 'NONE', #3534, #13409, #9796 ) ;
#15691 = CIRCLE ( 'NONE', #14680, 7.500000000000000000 ) ;
#15692 = LINE ( 'NONE', #12740, #5510 ) ;
#15693 = DIRECTION ( 'NONE',  ( 0.000000000000000000, 0.000000000000000000, -1.000000000000000000 ) ) ;
#15694 = AXIS2_PLACEMENT_3D ( 'NONE', #18050, #3324, #16350 ) ;
#15695 = EDGE_CURVE ( 'NONE', #16351, #19634, #9939, .T. ) ;
#15696 = VECTOR ( 'NONE', #11073, 1000.000000000000000 ) ;
#15697 = CARTESIAN_POINT ( 'NONE',  ( -6.929096494179677101, -2.870125741905209527, -23.77776249981969414 ) ) ;
#15698 = CARTESIAN_POINT ( 'NONE',  ( -30.00000000000000000, -85.00000000000000000, -11.50000000000000711 ) ) ;
#15699 = CARTESIAN_POINT ( 'NONE',  ( 19.99999999999999645, -15.58726123847806200, -62.93731870009420959 ) ) ;
#15700 = LINE ( 'NONE', #15590, #16120 ) ;
#15701 = VECTOR ( 'NONE', #9555, 1000.000000000000000 ) ;
#15702 = ADVANCED_FACE ( 'NONE', ( #9756 ), #11452, .F. ) ;
#15703 = CIRCLE ( 'NONE', #10289, 2.099999999999997868 ) ;
#15704 = VERTEX_POINT ( 'NONE', #11648 ) ;
#15705 = CARTESIAN_POINT ( 'NONE',  ( 18.00000000000000000, 0.000000000000000000, -130.0000000000000000 ) ) ;
#15706 = EDGE_CURVE ( 'NONE', #10182, #9751, #5531, .T. ) ;
#15707 = EDGE_LOOP ( 'NONE', ( #4007, #17481, #641, #9108, #13439, #8654 ) ) ;
#15708 = CARTESIAN_POINT ( 'NONE',  ( -10.19618095414378622, -15.25966316918061416, -22.48120624981968874 ) ) ;
#15709 = CARTESIAN_POINT ( 'NONE',  ( 15.62350230547613528, -14.77425901644551764, 73.92464627053533377 ) ) ;
#15710 = EDGE_LOOP ( 'NONE', ( #5474, #15892, #5193, #12881 ) ) ;
#15711 = CARTESIAN_POINT ( 'NONE',  ( 0.000000000000000000, 0.000000000000000000, 0.000000000000000000 ) ) ;
#15712 = ORIENTED_EDGE ( 'NONE', *, *, #3400, .F. ) ;
#15713 = DIRECTION ( 'NONE',  ( 0.000000000000000000, -0.1361666490962330778, -0.9906859460363326431 ) ) ;
#15714 = DIRECTION ( 'NONE',  ( 0.000000000000000000, 0.9790840876823234673, -0.2034560130526309185 ) ) ;
#15715 = DIRECTION ( 'NONE',  ( 0.000000000000000000, 0.000000000000000000, -1.000000000000000000 ) ) ;
#15716 = EDGE_CURVE ( 'NONE', #19211, #20725, #104, .T. ) ;
#15717 = AXIS2_PLACEMENT_3D ( 'NONE', #5863, #2269, #5748 ) ;
#15718 = ORIENTED_EDGE ( 'NONE', *, *, #5770, .T. ) ;
#15719 = FACE_BOUND ( 'NONE', #17073, .T. ) ;
#15720 = CARTESIAN_POINT ( 'NONE',  ( 48.35276434571220250, -3.649167310370820871, 90.00000000000000000 ) ) ;
#15721 = DIRECTION ( 'NONE',  ( 0.000000000000000000, -0.5000000000000011102, -0.8660254037844379305 ) ) ;
#15722 = AXIS2_PLACEMENT_3D ( 'NONE', #17855, #9685, #3323 ) ;
#15723 = DIRECTION ( 'NONE',  ( 0.000000000000000000, 0.000000000000000000, 1.000000000000000000 ) ) ;
#15724 = CIRCLE ( 'NONE', #20107, 27.60000000002759890 ) ;
#15725 = FACE_OUTER_BOUND ( 'NONE', #226, .T. ) ;
#15726 = VERTEX_POINT ( 'NONE', #8259 ) ;
#15727 = EDGE_CURVE ( 'NONE', #4659, #13626, #14432, .T. ) ;
#15728 = DIRECTION ( 'NONE',  ( 0.000000000000000000, 0.000000000000000000, -1.000000000000000000 ) ) ;
#15729 = CARTESIAN_POINT ( 'NONE',  ( 0.000000000000000000, -28.84646472442415543, -58.52617768068463278 ) ) ;
#15730 = ORIENTED_EDGE ( 'NONE', *, *, #10127, .T. ) ;
#15731 = DIRECTION ( 'NONE',  ( -0.000000000000000000, -0.000000000000000000, -1.000000000000000000 ) ) ;
#15732 = DIRECTION ( 'NONE',  ( 0.000000000000000000, -1.541976423090495387E-16, 1.000000000000000000 ) ) ;
#15733 = VERTEX_POINT ( 'NONE', #5073 ) ;
#15734 = CARTESIAN_POINT ( 'NONE',  ( -12.72792206288791128, -12.72792205982779912, -10.85707499981969093 ) ) ;
#15735 = EDGE_CURVE ( 'NONE', #19592, #1298, #19389, .T. ) ;
#15736 = CARTESIAN_POINT ( 'NONE',  ( -30.00000000000000000, -164.9999999999999716, 50.00000000000001421 ) ) ;
#15737 = LINE ( 'NONE', #19023, #14021 ) ;
#15738 = ORIENTED_EDGE ( 'NONE', *, *, #7035, .F. ) ;
#15739 = DIRECTION ( 'NONE',  ( 0.000000000000000000, 0.000000000000000000, 1.000000000000000000 ) ) ;
#15740 = ORIENTED_EDGE ( 'NONE', *, *, #4313, .F. ) ;
#15741 = AXIS2_PLACEMENT_3D ( 'NONE', #13096, #16681, #1962 ) ;
#15742 = DIRECTION ( 'NONE',  ( 0.000000000000000000, 0.000000000000000000, 1.000000000000000000 ) ) ;
#15743 = ORIENTED_EDGE ( 'NONE', *, *, #7411, .F. ) ;
#15744 = AXIS2_PLACEMENT_3D ( 'NONE', #16091, #4645, #1582 ) ;
#15745 = CARTESIAN_POINT ( 'NONE',  ( 33.70821056661568349, -116.6086985776691876, 76.50504368702979718 ) ) ;
#15746 = DIRECTION ( 'NONE',  ( 0.000000000000000000, 0.000000000000000000, 1.000000000000000000 ) ) ;
#15747 = CONTEXT_DEPENDENT_SHAPE_REPRESENTATION ( #6687, #16587 ) ;
#15748 = CARTESIAN_POINT ( 'NONE',  ( -14.79893867722910628, 2.943691928843437111, -7.527676831158455428 ) ) ;
#15749 = ORIENTED_EDGE ( 'NONE', *, *, #1740, .T. ) ;
#15750 = AXIS2_PLACEMENT_3D ( 'NONE', #18809, #16788, #5435 ) ;
#15751 = CARTESIAN_POINT ( 'NONE',  ( 0.000000000000000000, 27.62776854598936538, -58.65812137498974721 ) ) ;
#15752 = ORIENTED_EDGE ( 'NONE', *, *, #16961, .F. ) ;
#15753 = CARTESIAN_POINT ( 'NONE',  ( -5.303300859536632217, -5.303300858261584594, -24.36682499981969841 ) ) ;
#15754 = CARTESIAN_POINT ( 'NONE',  ( -12.72792206288790950, -12.72792205982779556, 15.51332500018031268 ) ) ;
#15755 = CARTESIAN_POINT ( 'NONE',  ( 7.500000000000004441, -8.788009009181406898E-15, -18.47619999999769647 ) ) ;
#15756 = LINE ( 'NONE', #12580, #12414 ) ;
#15757 = ORIENTED_EDGE ( 'NONE', *, *, #9769, .T. ) ;
#15758 = AXIS2_PLACEMENT_3D ( 'NONE', #4159, #10642, #15923 ) ;
#15759 = DIRECTION ( 'NONE',  ( 0.000000000000000000, 0.000000000000000000, 1.000000000000000000 ) ) ;
#15760 = DIRECTION ( 'NONE',  ( 0.000000000000000000, 0.000000000000000000, 1.000000000000000000 ) ) ;
#15761 = VERTEX_POINT ( 'NONE', #13042 ) ;
#15762 = CARTESIAN_POINT ( 'NONE',  ( 17.42669362192176052, -15.01422997234079126, -79.66264582819448492 ) ) ;
#15763 = EDGE_CURVE ( 'NONE', #3682, #8629, #12940, .T. ) ;
#15764 = VECTOR ( 'NONE', #9343, 1000.000000000000000 ) ;
#15765 = LINE ( 'NONE', #1266, #17126 ) ;
#15766 = CARTESIAN_POINT ( 'NONE',  ( 3.580422614997667896, 17.99999999956958163, -8.932768749819693710 ) ) ;
#15767 = EDGE_CURVE ( 'NONE', #4451, #19589, #2839, .T. ) ;
#15768 = ORIENTED_EDGE ( 'NONE', *, *, #433, .F. ) ;
#15769 = CARTESIAN_POINT ( 'NONE',  ( 19.99999999999999645, -62.46228066917801414, 18.86519267363435048 ) ) ;
#15770 = DIRECTION ( 'NONE',  ( 0.000000000000000000, 0.000000000000000000, -1.000000000000000000 ) ) ;
#15771 = FACE_OUTER_BOUND ( 'NONE', #4058, .T. ) ;
#15772 = DIRECTION ( 'NONE',  ( 0.000000000000000000, -0.9422609221188167350, -0.3348796121709969875 ) ) ;
#15773 = DIRECTION ( 'NONE',  ( 0.1301338387963445475, 0.9914964367057137462, 1.243481486083095525E-31 ) ) ;
#15774 = CARTESIAN_POINT ( 'NONE',  ( -15.25966317163203456, -10.19618095047498230, -1.137543749819690087 ) ) ;
#15775 = FACE_BOUND ( 'NONE', #14053, .T. ) ;
#15776 = VERTEX_POINT ( 'NONE', #17920 ) ;
#15777 = DIRECTION ( 'NONE',  ( -1.000000000000000000, -0.000000000000000000, 0.000000000000000000 ) ) ;
#15778 = AXIS2_PLACEMENT_3D ( 'NONE', #593, #17441, #10965 ) ;
#15779 = AXIS2_PLACEMENT_3D ( 'NONE', #7378, #2220, #6980 ) ;
#15780 = CARTESIAN_POINT ( 'NONE',  ( -2.943691925285395694, 14.79893867793683349, 7.471426831519076828 ) ) ;
#15781 = ORIENTED_EDGE ( 'NONE', *, *, #9285, .T. ) ;
#15782 = CARTESIAN_POINT ( 'NONE',  ( 19.99999999999999645, 31.98952867950324830, 56.39803944231596944 ) ) ;
#15783 = AXIS2_PLACEMENT_3D ( 'NONE', #10884, #2721, #13966 ) ;
#15784 = FACE_BOUND ( 'NONE', #8767, .T. ) ;
#15785 = DIRECTION ( 'NONE',  ( 1.000000000000000000, 0.000000000000000000, 0.000000000000000000 ) ) ;
#15786 = ORIENTED_EDGE ( 'NONE', *, *, #11479, .T. ) ;
#15787 = DIRECTION ( 'NONE',  ( 0.000000000000000000, 0.000000000000000000, 1.000000000000000000 ) ) ;
#15788 = AXIS2_PLACEMENT_3D ( 'NONE', #411, #14626, #9755 ) ;
#15789 = VERTEX_POINT ( 'NONE', #9846 ) ;
#15790 = DIRECTION ( 'NONE',  ( 0.000000000000000000, 0.7308359642781208088, 0.6825531432186576763 ) ) ;
#15791 = FACE_OUTER_BOUND ( 'NONE', #8444, .T. ) ;
#15792 = ORIENTED_EDGE ( 'NONE', *, *, #2227, .F. ) ;
#15793 = EDGE_LOOP ( 'NONE', ( #17148, #20181, #6402, #6907 ) ) ;
#15794 = CYLINDRICAL_SURFACE ( 'NONE', #9029, 50.00000000000001421 ) ;
#15795 = TOROIDAL_SURFACE ( 'NONE', #9034, 11.17999999999999439, 0.3200000000000012834 ) ;
#15796 = VECTOR ( 'NONE', #7458, 1000.000000000000114 ) ;
#15797 = FACE_OUTER_BOUND ( 'NONE', #10460, .T. ) ;
#15798 = EDGE_CURVE ( 'NONE', #18686, #5413, #4866, .T. ) ;
#15799 = AXIS2_PLACEMENT_3D ( 'NONE', #11154, #9358, #15715 ) ;
#15800 = FACE_OUTER_BOUND ( 'NONE', #18218, .T. ) ;
#15801 = CARTESIAN_POINT ( 'NONE',  ( -4.276731815070949239, -10.32494394706616347, -8.837077749352573619 ) ) ;
#15802 = CARTESIAN_POINT ( 'NONE',  ( -2.870125743571140919, -6.929096493489624642, -24.95588749981968846 ) ) ;
#15803 = CIRCLE ( 'NONE', #19199, 27.60000000002759890 ) ;
#15804 = CARTESIAN_POINT ( 'NONE',  ( 50.00000000000000000, 4.299168419249259188, 82.52564090190563206 ) ) ;
#15805 = CYLINDRICAL_SURFACE ( 'NONE', #10115, 65.24900000006525147 ) ;
#15806 = DIRECTION ( 'NONE',  ( 0.000000000000000000, 0.000000000000000000, 1.000000000000000000 ) ) ;
#15807 = EDGE_CURVE ( 'NONE', #18058, #2005, #16313, .T. ) ;
#15808 = AXIS2_PLACEMENT_3D ( 'NONE', #17035, #20421, #14187 ) ;
#15809 = ORIENTED_EDGE ( 'NONE', *, *, #20864, .F. ) ;
#15810 = VECTOR ( 'NONE', #2425, 1000.000000000000000 ) ;
#15811 = DIRECTION ( 'NONE',  ( 0.000000000000000000, 0.000000000000000000, 1.000000000000000000 ) ) ;
#15812 = ORIENTED_EDGE ( 'NONE', *, *, #19971, .F. ) ;
#15813 = CARTESIAN_POINT ( 'NONE',  ( 6.888301780572507305, -16.62983158603121936, -14.52886249981968625 ) ) ;
#15814 = CARTESIAN_POINT ( 'NONE',  ( 19.79075590726360900, -8.422956900484626530, 78.26370100276548669 ) ) ;
#15815 = ORIENTED_EDGE ( 'NONE', *, *, #7338, .F. ) ;
#15816 = CARTESIAN_POINT ( 'NONE',  ( 0.000000000000000000, 0.000000000000000000, -5.600000000000000533 ) ) ;
#15817 = ORIENTED_EDGE ( 'NONE', *, *, #808, .T. ) ;
#15818 = LINE ( 'NONE', #20680, #13226 ) ;
#15819 = CARTESIAN_POINT ( 'NONE',  ( 4.000000000000003553, 2.309401076758524685, -5.242734410091827613 ) ) ;
#15820 = CARTESIAN_POINT ( 'NONE',  ( 30.00000000000000000, -85.00000000000000000, -1.040949779275250179E-14 ) ) ;
#15821 = VECTOR ( 'NONE', #3063, 1000.000000000000000 ) ;
#15822 = ORIENTED_EDGE ( 'NONE', *, *, #20027, .F. ) ;
#15823 = DIRECTION ( 'NONE',  ( -1.000000000000000000, 0.000000000000000000, 0.000000000000000000 ) ) ;
#15824 = AXIS2_PLACEMENT_3D ( 'NONE', #16262, #17764, #4719 ) ;
#15825 = FACE_OUTER_BOUND ( 'NONE', #16632, .T. ) ;
#15826 = CARTESIAN_POINT ( 'NONE',  ( 6.888301780572505528, -16.62983158603121581, -23.95386249981969229 ) ) ;
#15827 = LINE ( 'NONE', #17315, #19117 ) ;
#15828 = EDGE_CURVE ( 'NONE', #12190, #10418, #12678, .T. ) ;
#15829 = VECTOR ( 'NONE', #4373, 1000.000000000000000 ) ;
#15830 = CIRCLE ( 'NONE', #15441, 54.99999999999999289 ) ;
#15831 = EDGE_CURVE ( 'NONE', #10418, #15600, #19418, .T. ) ;
#15832 = DIRECTION ( 'NONE',  ( -1.000000000000000000, -0.000000000000000000, 0.000000000000000000 ) ) ;
#15833 = VERTEX_POINT ( 'NONE', #17819 ) ;
#15834 = LINE ( 'NONE', #7987, #6601 ) ;
#15835 = EDGE_CURVE ( 'NONE', #17178, #17883, #14372, .T. ) ;
#15836 = DIRECTION ( 'NONE',  ( -1.000000000000000000, -0.000000000000000000, -0.000000000000000000 ) ) ;
#15837 = ORIENTED_EDGE ( 'NONE', *, *, #17899, .T. ) ;
#15838 = AXIS2_PLACEMENT_3D ( 'NONE', #15505, #20154, #16777 ) ;
#15839 = DIRECTION ( 'NONE',  ( 0.000000000000000000, 0.9790840876823220240, 0.2034560130526376631 ) ) ;
#15840 = CARTESIAN_POINT ( 'NONE',  ( 19.99999999999999645, -45.48683723007179225, -46.78012013466265273 ) ) ;
#15841 = PRODUCT_DEFINITION ( 'UNKNOWN', '', #7973, #16843 ) ;
#15842 = VERTEX_POINT ( 'NONE', #3477 ) ;
#15843 = CARTESIAN_POINT ( 'NONE',  ( 6.888301784570728614, 16.62983158437510056, -6.733637499819689509 ) ) ;
#15844 = DIRECTION ( 'NONE',  ( 0.000000000000000000, 0.000000000000000000, 1.000000000000000000 ) ) ;
#15845 = DIRECTION ( 'NONE',  ( 0.000000000000000000, 0.000000000000000000, -1.000000000000000000 ) ) ;
#15846 = ORIENTED_EDGE ( 'NONE', *, *, #2503, .T. ) ;
#15847 = DIRECTION ( 'NONE',  ( -1.000000000000000000, 0.000000000000000000, 0.000000000000000000 ) ) ;
#15848 = ORIENTED_EDGE ( 'NONE', *, *, #8210, .T. ) ;
#15849 = CARTESIAN_POINT ( 'NONE',  ( 19.99999999999999645, 24.01204443665187327, 60.22865198596132785 ) ) ;
#15850 = EDGE_CURVE ( 'NONE', #14887, #18615, #6876, .T. ) ;
#15851 = EDGE_LOOP ( 'NONE', ( #8252, #9750, #6581, #18927 ) ) ;
#15852 = EDGE_CURVE ( 'NONE', #297, #3604, #11635, .T. ) ;
#15853 = CARTESIAN_POINT ( 'NONE',  ( 2.500000000000000000, 2.357898499370431722, -2.818925648462311528E-15 ) ) ;
#15854 = EDGE_CURVE ( 'NONE', #18811, #8415, #13191, .T. ) ;
#15855 = DIRECTION ( 'NONE',  ( 1.000000000000000000, 0.000000000000000000, 0.000000000000000000 ) ) ;
#15856 = ITEM_DEFINED_TRANSFORMATION ( 'NONE', 'NONE', #11348,  #12461 ) ;
#15857 = CARTESIAN_POINT ( 'NONE',  ( 14.79893867793684059, 2.943691925285398359, -3.404239331158455339 ) ) ;
#15858 = ORIENTED_EDGE ( 'NONE', *, *, #18229, .T. ) ;
#15859 = CARTESIAN_POINT ( 'NONE',  ( -6.358192988180015881, -4.248408729364577141, -14.64729374981969379 ) ) ;
#15860 = CARTESIAN_POINT ( 'NONE',  ( 150.0000507999999968, 0.000000000000000000, 4.000000000000000000 ) ) ;
#15861 = ORIENTED_EDGE ( 'NONE', *, *, #5075, .F. ) ;
#15862 = CARTESIAN_POINT ( 'NONE',  ( 10.50529598519903729, -18.76196791309047640, 77.41653794407623934 ) ) ;
#15863 = DIRECTION ( 'NONE',  ( 0.000000000000000000, 0.000000000000000000, -1.000000000000000000 ) ) ;
#15864 = CARTESIAN_POINT ( 'NONE',  ( 30.00000000000000000, -159.9999999999999716, 53.99496054166689873 ) ) ;
#15865 = VERTEX_POINT ( 'NONE', #16619 ) ;
#15866 = CARTESIAN_POINT ( 'NONE',  ( 8.900000000000046541, 10.82531754730546147, 126.0000000000000000 ) ) ;
#15867 = DIRECTION ( 'NONE',  ( -1.000000000000000000, -0.000000000000000000, -0.000000000000000000 ) ) ;
#15868 = ORIENTED_EDGE ( 'NONE', *, *, #20511, .T. ) ;
#15869 = CYLINDRICAL_SURFACE ( 'NONE', #17364, 72.00000000007199219 ) ;
#15870 = DIRECTION ( 'NONE',  ( -0.000000000000000000, -0.000000000000000000, 1.000000000000000000 ) ) ;
#15871 = CARTESIAN_POINT ( 'NONE',  ( -12.72792205982779556, 12.72792206288790773, -10.40542499981968838 ) ) ;
#15872 = EDGE_LOOP ( 'NONE', ( #16572, #2794 ) ) ;
#15873 = CARTESIAN_POINT ( 'NONE',  ( 1.491842754445843688, -7.500000000179346316, -10.14958124981968268 ) ) ;
#15874 = DIRECTION ( 'NONE',  ( -1.000000000000000000, -0.000000000000000000, 0.000000000000000000 ) ) ;
#15875 = FACE_OUTER_BOUND ( 'NONE', #2611, .T. ) ;
#15876 = DIRECTION ( 'NONE',  ( 1.000000000000000000, 0.000000000000000000, 0.000000000000000000 ) ) ;
#15877 = CARTESIAN_POINT ( 'NONE',  ( -10.00000000000000178, -85.00000000000000000, -1.040949779275250179E-14 ) ) ;
#15878 = CARTESIAN_POINT ( 'NONE',  ( 18.00000000043041481, 3.580422610670020322, 4.164018750180309425 ) ) ;
#15879 = CARTESIAN_POINT ( 'NONE',  ( 2.870125743571140475, 6.929096493489632635, -13.97848749981969085 ) ) ;
#15880 = ORIENTED_EDGE ( 'NONE', *, *, #693, .F. ) ;
#15881 = CIRCLE ( 'NONE', #2340, 27.60000000002759890 ) ;
#15882 = LINE ( 'NONE', #9519, #17180 ) ;
#15883 = CARTESIAN_POINT ( 'NONE',  ( -1.343452921478823292E-09, -11.17563879731704723, -25.97385975028680605 ) ) ;
#15884 = EDGE_CURVE ( 'NONE', #5471, #13088, #15364, .T. ) ;
#15885 = CYLINDRICAL_SURFACE ( 'NONE', #6768, 2.099999999999999645 ) ;
#15886 = ORIENTED_EDGE ( 'NONE', *, *, #10864, .F. ) ;
#15887 = DIRECTION ( 'NONE',  ( 0.000000000000000000, 0.000000000000000000, 1.000000000000000000 ) ) ;
#15888 = CARTESIAN_POINT ( 'NONE',  ( -17.99999999956958519, 3.580422614997674113, -18.80941874981968809 ) ) ;
#15889 = CARTESIAN_POINT ( 'NONE',  ( 49.35000000000000142, -99.99999999999998579, 5.000000000000000000 ) ) ;
#15890 = EDGE_LOOP ( 'NONE', ( #3401, #6071 ) ) ;
#15891 = PLANE ( 'NONE',  #12617 ) ;
#15892 = ORIENTED_EDGE ( 'NONE', *, *, #16344, .T. ) ;
#15893 = CARTESIAN_POINT ( 'NONE',  ( 49.35000000000000142, -39.99999999999999289, 0.000000000000000000 ) ) ;
#15894 = DIRECTION ( 'NONE',  ( 1.000000000000000000, 0.000000000000000000, 0.000000000000000000 ) ) ;
#15895 = VERTEX_POINT ( 'NONE', #18432 ) ;
#15896 = EDGE_LOOP ( 'NONE', ( #10220, #4299 ) ) ;
#15897 = CARTESIAN_POINT ( 'NONE',  ( -15.15000000000000568, 3.245314017740485469E-16, 40.00000000000000000 ) ) ;
#15898 = AXIS2_PLACEMENT_3D ( 'NONE', #19869, #1759, #16178 ) ;
#15899 =( LENGTH_UNIT ( ) NAMED_UNIT ( * ) SI_UNIT ( .MILLI., .METRE. ) );
#15900 = CYLINDRICAL_SURFACE ( 'NONE', #5173, 65.24900000006525147 ) ;
#15901 = DIRECTION ( 'NONE',  ( 0.000000000000000000, 0.000000000000000000, -1.000000000000000000 ) ) ;
#15902 = CARTESIAN_POINT ( 'NONE',  ( -4.276731812588566939, 10.32494394809439875, -14.72770274935257362 ) ) ;
#15903 =( BOUNDED_CURVE ( )  B_SPLINE_CURVE ( 2, ( #4583, #19383, #16211, #12836, #1894, #5065, #13035, #6445, #18004, #19687, #12933, #5167, #18111, #4871, #16000, #1502, #17811, #6553, #3281, #9749, #19489, #10366, #19793, #6857, #16833, #16928, #5275, #18312, #3886, #13654, #5581, #12061, #3779, #18217, #3993, #11748, #7067, #3681, #10473, #13760, #10055, #20212, #11950, #8870, #10155, #832, #2204, #10260, #16722, #16610, #8765, #18532, #8661, #15136, #15344, #5689, #2410, #2100, #404, #20103, #623, #8556, #15036, #11845, #518, #12161, #13547, #18628, #19992, #2003, #5476, #18424, #6964, #2313, #16519, #13452, #8452, #19901, #15234, #716, #14928, #7173, #7280, #5377, #13347, #7488, #6112, #10795, #5911, #13972, #1154, #20733, #20428, #18952, #14084, #4422, #9415, #17152, #2638, #14289, #7605, #13863, #12382, #15766, #6218, #1367, #18744, #6018, #15871, #17041, #19055, #9195, #14192, #12490, #15546, #1042, #2529, #5792, #7813, #18850, #12588, #9096, #4327, #12706, #20535, #20310, #4092, #9303, #8986, #17256, #15452, #2726, #15656, #7719, #10888, #17362, #943, #2835, #12268, #1267, #10578, #20635, #7386, #4215, #10692, #4531, #10994, #17471, #2947, #19161, #13115, #4740, #9720, #174, #4948, #13013, #11206, #20844, #19568, #16281, #4638 ),
 .UNSPECIFIED., .F., .T. ) 
 B_SPLINE_CURVE_WITH_KNOTS ( ( 3, 2, 2, 2, 2, 2, 2, 2, 2, 2, 2, 2, 2, 2, 2, 2, 2, 2, 2, 2, 2, 2, 2, 2, 2, 2, 2, 2, 2, 2, 2, 2, 2, 2, 2, 2, 2, 2, 2, 2, 2, 2, 2, 2, 2, 2, 2, 2, 2, 2, 2, 2, 2, 2, 2, 2, 2, 2, 2, 2, 2, 2, 2, 2, 2, 2, 2, 2, 2, 2, 2, 2, 2, 2, 2, 2, 2, 2, 2, 2, 3 ),
 ( 0.000000000000000000, 0.01250000000000000069, 0.02500000000000000139, 0.03749999999999999861, 0.05000000000000000278, 0.06250000000000000000, 0.07499999999999999722, 0.08749999999999999445, 0.1000000000000000056, 0.1125000000000000028, 0.1250000000000000000, 0.1375000000000000111, 0.1499999999999999944, 0.1625000000000000056, 0.1749999999999999889, 0.1875000000000000000, 0.2000000000000000111, 0.2124999999999999944, 0.2250000000000000056, 0.2374999999999999889, 0.2500000000000000000, 0.2625000000000000111, 0.2750000000000000222, 0.2874999999999999778, 0.2999999999999999889, 0.3125000000000000000, 0.3250000000000000111, 0.3375000000000000222, 0.3499999999999999778, 0.3624999999999999889, 0.3750000000000000000, 0.3875000000000000111, 0.4000000000000000222, 0.4124999999999999778, 0.4249999999999999889, 0.4375000000000000000, 0.4500000000000000111, 0.4625000000000000222, 0.4749999999999999778, 0.4874999999999999889, 0.5000000000000000000, 0.5124999999999999556, 0.5250000000000000222, 0.5374999999999999778, 0.5500000000000000444, 0.5625000000000000000, 0.5749999999999999556, 0.5875000000000000222, 0.5999999999999999778, 0.6125000000000000444, 0.6250000000000000000, 0.6374999999999999556, 0.6500000000000000222, 0.6624999999999999778, 0.6750000000000000444, 0.6875000000000000000, 0.6999999999999999556, 0.7125000000000000222, 0.7249999999999999778, 0.7375000000000000444, 0.7500000000000000000, 0.7624999999999999556, 0.7750000000000000222, 0.7874999999999999778, 0.8000000000000000444, 0.8125000000000000000, 0.8249999999999999556, 0.8375000000000000222, 0.8499999999999999778, 0.8625000000000000444, 0.8750000000000000000, 0.8874999999999999556, 0.9000000000000000222, 0.9124999999999999778, 0.9250000000000000444, 0.9375000000000000000, 0.9499999999999999556, 0.9625000000000000222, 0.9749999999999999778, 0.9875000000000000444, 1.000000000000000000 ),
 .UNSPECIFIED. ) 
 CURVE ( )  GEOMETRIC_REPRESENTATION_ITEM ( )  RATIONAL_B_SPLINE_CURVE ( ( 1.000000000000000000, 0.9807852804032304306, 1.000000000000000000, 0.9807852804032304306, 1.000000000000000000, 0.9807852804032304306, 1.000000000000000000, 0.9807852804032304306, 1.000000000000000000, 0.9807852804032304306, 1.000000000000000000, 0.9807852804032304306, 1.000000000000000000, 0.9807852804032304306, 1.000000000000000000, 0.9807852804032304306, 1.000000000000000000, 0.9807852804032304306, 1.000000000000000000, 0.9807852804032304306, 1.000000000000000000, 0.9807852804032304306, 1.000000000000000000, 0.9807852804032304306, 1.000000000000000000, 0.9807852804032304306, 1.000000000000000000, 0.9807852804032304306, 1.000000000000000000, 0.9807852804032304306, 1.000000000000000000, 0.9807852804032304306, 1.000000000000000000, 0.9807852804032304306, 1.000000000000000000, 0.9807852804032304306, 1.000000000000000000, 0.9807852804032304306, 1.000000000000000000, 0.9807852804032304306, 1.000000000000000000, 0.9807852804032304306, 1.000000000000000000, 0.9807852804032304306, 1.000000000000000000, 0.9807852804032304306, 1.000000000000000000, 0.9807852804032304306, 1.000000000000000000, 0.9807852804032304306, 1.000000000000000000, 0.9807852804032304306, 1.000000000000000000, 0.9807852804032304306, 1.000000000000000000, 0.9807852804032304306, 1.000000000000000000, 0.9807852804032304306, 1.000000000000000000, 0.9807852804032304306, 1.000000000000000000, 0.9807852804032304306, 1.000000000000000000, 0.9807852804032304306, 1.000000000000000000, 0.9807852804032304306, 1.000000000000000000, 0.9807852804032304306, 1.000000000000000000, 0.9807852804032304306, 1.000000000000000000, 0.9807852804032304306, 1.000000000000000000, 0.9807852804032304306, 1.000000000000000000, 0.9807852804032304306, 1.000000000000000000, 0.9807852804032304306, 1.000000000000000000, 0.9807852804032304306, 1.000000000000000000, 0.9807852804032304306, 1.000000000000000000, 0.9807852804032304306, 1.000000000000000000, 0.9807852804032304306, 1.000000000000000000, 0.9807852804032304306, 1.000000000000000000, 0.9807852804032304306, 1.000000000000000000, 0.9807852804032304306, 1.000000000000000000, 0.9807852804032304306, 1.000000000000000000, 0.9807852804032304306, 1.000000000000000000, 0.9807852804032304306, 1.000000000000000000, 0.9807852804032304306, 1.000000000000000000, 0.9807852804032304306, 1.000000000000000000, 0.9807852804032304306, 1.000000000000000000, 0.9807852804032304306, 1.000000000000000000, 0.9807852804032304306, 1.000000000000000000, 0.9807852804032304306, 1.000000000000000000, 0.9807852804032304306, 1.000000000000000000, 0.9807852804032304306, 1.000000000000000000, 0.9807852804032304306, 1.000000000000000000, 0.9807852804032304306, 1.000000000000000000, 0.9807852804032304306, 1.000000000000000000, 0.9807852804032304306, 1.000000000000000000, 0.9807852804032304306, 1.000000000000000000, 0.9807852804032304306, 1.000000000000000000, 0.9807852804032304306, 1.000000000000000000, 0.9807852804032304306, 1.000000000000000000, 0.9807852804032304306, 1.000000000000000000, 0.9807852804032304306, 1.000000000000000000, 0.9807852804032304306, 1.000000000000000000, 0.9807852804032304306, 1.000000000000000000, 0.9807852804032304306, 1.000000000000000000, 0.9807852804032304306, 1.000000000000000000, 0.9807852804032304306, 1.000000000000000000, 0.9807852804032304306, 1.000000000000000000, 0.9807852804032304306, 1.000000000000000000, 0.9807852804032304306, 1.000000000000000000, 0.9807852804032304306, 1.000000000000000000, 0.9807852804032304306, 1.000000000000000000, 0.9807852804032304306, 1.000000000000000000, 0.9807852804032304306, 1.000000000000000000, 0.9807852804032304306, 1.000000000000000000 ) ) 
 REPRESENTATION_ITEM ( '' )  );
#15904 = CARTESIAN_POINT ( 'NONE',  ( 4.248408729364575365, -6.358192988180014993, -17.00354374981968775 ) ) ;
#15905 = ADVANCED_FACE ( 'NONE', ( #13355 ), #5383, .T. ) ;
#15906 = DIRECTION ( 'NONE',  ( 0.000000000000000000, 0.000000000000000000, -1.000000000000000000 ) ) ;
#15907 = DIRECTION ( 'NONE',  ( -1.000000000000000000, 0.000000000000000000, 0.000000000000000000 ) ) ;
#15908 = CARTESIAN_POINT ( 'NONE',  ( 0.000000000000000000, 63.05226888949891162, 15.11556105343481882 ) ) ;
#15909 = VERTEX_POINT ( 'NONE', #12071 ) ;
#15910 = DIRECTION ( 'NONE',  ( -0.000000000000000000, -0.000000000000000000, -1.000000000000000000 ) ) ;
#15911 = ORIENTED_EDGE ( 'NONE', *, *, #8242, .F. ) ;
#15912 = CARTESIAN_POINT ( 'NONE',  ( -12.72792206288791128, -12.72792205982779912, -22.18667499981969371 ) ) ;
#15913 = CARTESIAN_POINT ( 'NONE',  ( 20.42938063014384298, -6.725612673823795795, 79.66382435179508548 ) ) ;
#15914 = ORIENTED_EDGE ( 'NONE', *, *, #10331, .F. ) ;
#15915 = EDGE_CURVE ( 'NONE', #659, #13680, #5208, .T. ) ;
#15916 = DIRECTION ( 'NONE',  ( 1.000000000000000000, -1.734723475976807094E-16, 0.000000000000000000 ) ) ;
#15917 = ORIENTED_EDGE ( 'NONE', *, *, #4617, .T. ) ;
#15918 = CARTESIAN_POINT ( 'NONE',  ( 19.99999999999999645, 55.05624179292029652, -35.01774179823726740 ) ) ;
#15919 = DIRECTION ( 'NONE',  ( 0.000000000000000000, -0.000000000000000000, 1.000000000000000000 ) ) ;
#15920 = FACE_OUTER_BOUND ( 'NONE', #5000, .T. ) ;
#15921 = AXIS2_PLACEMENT_3D ( 'NONE', #7009, #8486, #18459 ) ;
#15922 = ORIENTED_EDGE ( 'NONE', *, *, #2562, .F. ) ;
#15923 = DIRECTION ( 'NONE',  ( -1.000000000000000000, 0.000000000000000000, 0.000000000000000000 ) ) ;
#15924 = DIRECTION ( 'NONE',  ( -1.000000000000000000, 0.000000000000000000, 0.000000000000000000 ) ) ;
#15925 = DIRECTION ( 'NONE',  ( 0.000000000000000000, 0.000000000000000000, 1.000000000000000000 ) ) ;
#15926 = CIRCLE ( 'NONE', #19640, 72.00000000007199219 ) ;
#15927 = DIRECTION ( 'NONE',  ( 0.000000000000000000, 0.000000000000000000, 1.000000000000000000 ) ) ;
#15928 = ORIENTED_EDGE ( 'NONE', *, *, #12075, .T. ) ;
#15929 = DIRECTION ( 'NONE',  ( -0.000000000000000000, 1.000000000000000000, 1.224646799147353207E-16 ) ) ;
#15930 = CARTESIAN_POINT ( 'NONE',  ( 2.870125741905214412, -6.929096494179682431, -1.019112499819684770 ) ) ;
#15931 = CIRCLE ( 'NONE', #6784, 2.099999999999990763 ) ;
#15932 = ORIENTED_EDGE ( 'NONE', *, *, #16035, .F. ) ;
#15933 = DIRECTION ( 'NONE',  ( 1.000000000000000000, 0.000000000000000000, 0.000000000000000000 ) ) ;
#15934 = DIRECTION ( 'NONE',  ( -1.000000000000000000, -0.000000000000000000, -0.000000000000000000 ) ) ;
#15935 = VERTEX_POINT ( 'NONE', #16525 ) ;
#15936 = FACE_OUTER_BOUND ( 'NONE', #7836, .T. ) ;
#15937 = LINE ( 'NONE', #1435, #19511 ) ;
#15938 = DIRECTION ( 'NONE',  ( 1.000000000000000000, 0.000000000000000000, 0.000000000000000000 ) ) ;
#15939 = ORIENTED_EDGE ( 'NONE', *, *, #13780, .T. ) ;
#15940 = ADVANCED_FACE ( 'NONE', ( #2319 ), #181, .F. ) ;
#15941 = CARTESIAN_POINT ( 'NONE',  ( 19.99999999999999645, -59.36728637277991538, -40.73727173906846843 ) ) ;
#15942 = EDGE_LOOP ( 'NONE', ( #10991, #5375, #968, #7798, #18563, #6610 ) ) ;
#15943 = CARTESIAN_POINT ( 'NONE',  ( 10.00000000000000178, -164.9999999999999716, -66.80000000000001137 ) ) ;
#15944 = ADVANCED_FACE ( 'NONE', ( #6029, #15775 ), #9107, .T. ) ;
#15945 = EDGE_LOOP ( 'NONE', ( #7199, #469, #18599, #5873 ) ) ;
#15946 = AXIS2_PLACEMENT_3D ( 'NONE', #3805, #10290, #16750 ) ;
#15947 = EDGE_CURVE ( 'NONE', #9919, #8092, #9767, .T. ) ;
#15948 = DIRECTION ( 'NONE',  ( -1.000000000000000000, 0.000000000000000000, -0.000000000000000000 ) ) ;
#15949 = CARTESIAN_POINT ( 'NONE',  ( 50.00000000000000000, 230.0000000000000000, 85.00000000000000000 ) ) ;
#15950 = CARTESIAN_POINT ( 'NONE',  ( 12.54593441562640876, -8.382925371439629458, -21.07611433115846111 ) ) ;
#15951 = ORIENTED_EDGE ( 'NONE', *, *, #8194, .T. ) ;
#15952 = CARTESIAN_POINT ( 'NONE',  ( 1.491842754445842578, -7.500000000179340987, -16.41448124981969059 ) ) ;
#15953 = LINE ( 'NONE', #12895, #19065 ) ;
#15954 = VERTEX_POINT ( 'NONE', #7500 ) ;
#15955 = AXIS2_PLACEMENT_3D ( 'NONE', #12635, #9443, #4457 ) ;
#15956 = CARTESIAN_POINT ( 'NONE',  ( 0.000000000000000000, -60.40676135667420965, -23.56039007469101421 ) ) ;
#15957 = EDGE_CURVE ( 'NONE', #12350, #4610, #14357, .T. ) ;
#15958 = AXIS2_PLACEMENT_3D ( 'NONE', #12898, #9711, #163 ) ;
#15959 = CARTESIAN_POINT ( 'NONE',  ( -4.248408729364577141, 6.358192988180014993, -21.71604374981969343 ) ) ;
#15960 = AXIS2_PLACEMENT_3D ( 'NONE', #14288, #6017, #4214 ) ;
#15961 = CARTESIAN_POINT ( 'NONE',  ( 6.165580000000000283, 0.000000000000000000, 0.000000000000000000 ) ) ;
#15962 = EDGE_CURVE ( 'NONE', #10605, #44, #14012, .T. ) ;
#15963 = ORIENTED_EDGE ( 'NONE', *, *, #8065, .T. ) ;
#15964 = ADVANCED_FACE ( 'NONE', ( #12602 ), #19067, .F. ) ;
#15965 = PLANE ( 'NONE',  #11753 ) ;
#15966 = CARTESIAN_POINT ( 'NONE',  ( -6.165580000000000283, 0.000000000000000000, 0.000000000000000000 ) ) ;
#15967 = AXIS2_PLACEMENT_3D ( 'NONE', #8914, #12422, #10826 ) ;
#15968 = ORIENTED_EDGE ( 'NONE', *, *, #2538, .T. ) ;
#15969 = FACE_OUTER_BOUND ( 'NONE', #13887, .T. ) ;
#15970 = CARTESIAN_POINT ( 'NONE',  ( -30.00000000000000000, -85.00000000000000000, -1.040949779275250179E-14 ) ) ;
#15971 = ADVANCED_FACE ( 'NONE', ( #19367, #4855 ), #1780, .F. ) ;
#15972 = CARTESIAN_POINT ( 'NONE',  ( 19.99999999999999645, 0.000000000000000000, 0.000000000000000000 ) ) ;
#15973 = ORIENTED_EDGE ( 'NONE', *, *, #5358, .F. ) ;
#15974 = DIRECTION ( 'NONE',  ( -1.000000000000000000, 0.000000000000000000, 0.000000000000000000 ) ) ;
#15975 = VECTOR ( 'NONE', #16059, 1000.000000000000000 ) ;
#15976 = AXIS2_PLACEMENT_3D ( 'NONE', #9345, #4256, #872 ) ;
#15977 = DIRECTION ( 'NONE',  ( 0.000000000000000000, -1.000000000000000000, 0.000000000000000000 ) ) ;
#15978 = DIRECTION ( 'NONE',  ( 1.000000000000000000, -0.000000000000000000, -0.000000000000000000 ) ) ;
#15979 = CIRCLE ( 'NONE', #13274, 11.50000000000000000 ) ;
#15980 = CARTESIAN_POINT ( 'NONE',  ( 42.00000000000000000, -85.00000000000000000, -1.040949779275250179E-14 ) ) ;
#15981 = CARTESIAN_POINT ( 'NONE',  ( -6.888301784570739272, -16.62983158437509701, -20.87113749981968880 ) ) ;
#15982 = EDGE_CURVE ( 'NONE', #2747, #5439, #9277, .T. ) ;
#15983 = CARTESIAN_POINT ( 'NONE',  ( 1.491842754445843688, -7.500000000179346316, -10.14958124981968268 ) ) ;
#15984 = FACE_OUTER_BOUND ( 'NONE', #17813, .T. ) ;
#15985 = EDGE_CURVE ( 'NONE', #10946, #125, #16198, .T. ) ;
#15986 = CARTESIAN_POINT ( 'NONE',  ( 8.382925371439627682, 12.54593441562639988, 8.649551831519074696 ) ) ;
#15987 = LINE ( 'NONE', #10508, #1724 ) ;
#15988 = VECTOR ( 'NONE', #16840, 1000.000000000000000 ) ;
#15989 = AXIS2_PLACEMENT_3D ( 'NONE', #10076, #10387, #1913 ) ;
#15990 = ORIENTED_EDGE ( 'NONE', *, *, #6397, .T. ) ;
#15991 = AXIS2_PLACEMENT_3D ( 'NONE', #4963, #14518, #8045 ) ;
#15992 = DIRECTION ( 'NONE',  ( -1.000000000000000000, -0.000000000000000000, -0.000000000000000000 ) ) ;
#15993 = CARTESIAN_POINT ( 'NONE',  ( 30.00000000000000000, -113.2094389508847314, -74.86138894033632596 ) ) ;
#15994 = CARTESIAN_POINT ( 'NONE',  ( 1.040949779275250179E-14, -85.00000000000000000, 5.000000000000000000 ) ) ;
#15995 = CIRCLE ( 'NONE', #6838, 10.85999999999999233 ) ;
#15996 = ORIENTED_EDGE ( 'NONE', *, *, #6233, .F. ) ;
#15997 = DIRECTION ( 'NONE',  ( 0.000000000000000000, -1.000000000000000000, 0.000000000000000000 ) ) ;
#15998 = ORIENTED_EDGE ( 'NONE', *, *, #4130, .T. ) ;
#15999 = CARTESIAN_POINT ( 'NONE',  ( 43.44798870043372574, -10.84402389218931795, -82.73379815179617935 ) ) ;
#16000 = CARTESIAN_POINT ( 'NONE',  ( -16.62983158437509701, 6.888301784570728614, 17.28051250018031126 ) ) ;
#16001 = ORIENTED_EDGE ( 'NONE', *, *, #12887, .T. ) ;
#16002 = VECTOR ( 'NONE', #17242, 1000.000000000000000 ) ;
#16003 = VERTEX_POINT ( 'NONE', #1685 ) ;
#16004 = CARTESIAN_POINT ( 'NONE',  ( 31.27203855688423673, -112.0327841679104495, -74.37803300064821599 ) ) ;
#16005 = EDGE_CURVE ( 'NONE', #10469, #8874, #11298, .T. ) ;
#16006 =( LENGTH_UNIT ( ) NAMED_UNIT ( * ) SI_UNIT ( .MILLI., .METRE. ) );
#16007 = DIRECTION ( 'NONE',  ( -1.202124453834178081E-10, -1.000000000000000000, 6.477240929643252887E-26 ) ) ;
#16008 = VECTOR ( 'NONE', #10455, 1000.000000000000000 ) ;
#16009 = AXIS2_PLACEMENT_3D ( 'NONE', #9278, #12355, #10970 ) ;
#16010 = AXIS2_PLACEMENT_3D ( 'NONE', #2669, #2870, #15693 ) ;
#16011 = DIRECTION ( 'NONE',  ( -0.000000000000000000, -0.000000000000000000, 1.000000000000000000 ) ) ;
#16013 = AXIS2_PLACEMENT_3D ( 'NONE', #15111, #19970, #600 ) ;
#16012 = CARTESIAN_POINT ( 'NONE',  ( -11.17563879731705789, 1.343452237168309506E-09, -16.49489024935257575 ) ) ;
#16014 = CARTESIAN_POINT ( 'NONE',  ( 10.32494394809438987, 4.276731812588564274, 18.20582774971320461 ) ) ;
#16015 = DIRECTION ( 'NONE',  ( 0.000000000000000000, 0.5195839500354344498, -0.8544194045464880150 ) ) ;
#16016 = CIRCLE ( 'NONE', #3815, 27.60000000002759890 ) ;
#16017 = DIRECTION ( 'NONE',  ( 0.000000000000000000, 0.9790840876823220240, 0.2034560130526374133 ) ) ;
#16018 = FACE_OUTER_BOUND ( 'NONE', #14426, .T. ) ;
#16019 = EDGE_LOOP ( 'NONE', ( #1311, #14004, #2353, #1284 ) ) ;
#16020 = CARTESIAN_POINT ( 'NONE',  ( 2.500000000000000000, -1.768423874527823791, -1.020999999999998353 ) ) ;
#16021 = VERTEX_POINT ( 'NONE', #4746 ) ;
#16022 = CARTESIAN_POINT ( 'NONE',  ( -17.99999999956958519, 3.580422614997674113, -11.28901874981968589 ) ) ;
#16023 = DIRECTION ( 'NONE',  ( 0.000000000000000000, 0.000000000000000000, -1.000000000000000000 ) ) ;
#16024 = VECTOR ( 'NONE', #6306, 1000.000000000000000 ) ;
#16025 = ORIENTED_EDGE ( 'NONE', *, *, #10367, .F. ) ;
#16026 = CIRCLE ( 'NONE', #6868, 0.2000000000000000944 ) ;
#16027 = DIRECTION ( 'NONE',  ( -1.734723475976807094E-16, -1.000000000000000000, 0.000000000000000000 ) ) ;
#16028 = ORIENTED_EDGE ( 'NONE', *, *, #2976, .T. ) ;
#16029 = DIRECTION ( 'NONE',  ( 0.000000000000000000, 0.000000000000000000, 1.000000000000000000 ) ) ;
#16030 = CARTESIAN_POINT ( 'NONE',  ( -4.000000000000000000, 2.309401076758496263, -5.599999999999999645 ) ) ;
#16031 = DIRECTION ( 'NONE',  ( 1.000000000000000000, -0.000000000000000000, -0.000000000000000000 ) ) ;
#16032 = EDGE_LOOP ( 'NONE', ( #8690, #16930, #10499, #17234 ) ) ;
#16033 = CARTESIAN_POINT ( 'NONE',  ( -30.00000000000000000, -97.49621075554985339, -111.6458212409894486 ) ) ;
#16034 = EDGE_CURVE ( 'NONE', #8981, #6083, #12998, .T. ) ;
#16035 = EDGE_CURVE ( 'NONE', #9551, #5163, #8247, .T. ) ;
#16036 = AXIS2_PLACEMENT_3D ( 'NONE', #6591, #7992, #6794 ) ;
#16037 = DIRECTION ( 'NONE',  ( -1.000000000000000000, -0.000000000000000000, -0.000000000000000000 ) ) ;
#16038 = DIRECTION ( 'NONE',  ( 1.000000000000000000, 0.000000000000000000, 0.000000000000000000 ) ) ;
#16039 = AXIS2_PLACEMENT_3D ( 'NONE', #12841, #1804, #19285 ) ;
#16040 = AXIS2_PLACEMENT_3D ( 'NONE', #9269, #4707, #4492 ) ;
#16041 = CARTESIAN_POINT ( 'NONE',  ( -9.015947181032828388E-10, -7.500000000000002665, 12.15505000018031012 ) ) ;
#16042 = CIRCLE ( 'NONE', #9926, 27.60000000002759890 ) ;
#16044 = ORIENTED_EDGE ( 'NONE', *, *, #16077, .F. ) ;
#16043 = AXIS2_PLACEMENT_3D ( 'NONE', #17094, #2680, #13915 ) ;
#16045 = CARTESIAN_POINT ( 'NONE',  ( 0.000000000000000000, -56.63599015375694989, 31.56633360682443268 ) ) ;
#16046 = CARTESIAN_POINT ( 'NONE',  ( 40.00000000000000711, -30.00000000000001421, -120.0000000000000142 ) ) ;
#16047 = ORIENTED_EDGE ( 'NONE', *, *, #12819, .F. ) ;
#16048 = DIRECTION ( 'NONE',  ( 0.000000000000000000, -1.000000000000000000, -8.673617379884036705E-17 ) ) ;
#16049 = CYLINDRICAL_SURFACE ( 'NONE', #6873, 27.60000000002759890 ) ;
#16050 = ORIENTED_EDGE ( 'NONE', *, *, #19971, .T. ) ;
#16051 = DIRECTION ( 'NONE',  ( 1.000000000000000000, 0.000000000000000000, 0.000000000000000000 ) ) ;
#16052 = CYLINDRICAL_SURFACE ( 'NONE', #19838, 72.00000000007199219 ) ;
#16053 = FACE_OUTER_BOUND ( 'NONE', #1309, .T. ) ;
#16054 = AXIS2_PLACEMENT_3D ( 'NONE', #1641, #9778, #10089 ) ;
#16055 = ORIENTED_EDGE ( 'NONE', *, *, #6272, .F. ) ;
#16056 = AXIS2_PLACEMENT_3D ( 'NONE', #1250, #7797, #12473 ) ;
#16057 = DIRECTION ( 'NONE',  ( -1.000000000000000000, 0.000000000000000000, -0.000000000000000000 ) ) ;
#16058 = EDGE_LOOP ( 'NONE', ( #2351, #6162, #15302, #4846 ) ) ;
#16059 = DIRECTION ( 'NONE',  ( -1.000000000000000000, 0.000000000000000000, 0.000000000000000000 ) ) ;
#16060 = VERTEX_POINT ( 'NONE', #6537 ) ;
#16061 = AXIS2_PLACEMENT_3D ( 'NONE', #14770, #252, #11582 ) ;
#16062 = FACE_OUTER_BOUND ( 'NONE', #6243, .T. ) ;
#16063 = CARTESIAN_POINT ( 'NONE',  ( -26.35784117651625280, 26.35784117651607872, -130.0000000000000000 ) ) ;
#16064 = CARTESIAN_POINT ( 'NONE',  ( -2.943691925285397470, 14.79893867793684059, -15.18548933115845401 ) ) ;
#16065 = EDGE_CURVE ( 'NONE', #10739, #1628, #5051, .T. ) ;
#16066 = EDGE_CURVE ( 'NONE', #4449, #17301, #20083, .T. ) ;
#16067 = ORIENTED_EDGE ( 'NONE', *, *, #14826, .F. ) ;
#16068 = CARTESIAN_POINT ( 'NONE',  ( 0.000000000000000000, 0.000000000000000000, 0.000000000000000000 ) ) ;
#16069 = EDGE_CURVE ( 'NONE', #18310, #2694, #6222, .T. ) ;
#16070 = DIRECTION ( 'NONE',  ( -1.000000000000000000, -0.000000000000000000, -0.000000000000000000 ) ) ;
#16071 = ORIENTED_EDGE ( 'NONE', *, *, #8476, .F. ) ;
#16072 = CARTESIAN_POINT ( 'NONE',  ( 15.54275544017199628, -14.85857375444459905, 79.76610145095158089 ) ) ;
#16073 = CIRCLE ( 'NONE', #9648, 20.00000000000000355 ) ;
#16074 = DIRECTION ( 'NONE',  ( 0.000000000000000000, 0.000000000000000000, 1.000000000000000000 ) ) ;
#16075 = DIRECTION ( 'NONE',  ( 1.000000000000000000, 0.000000000000000000, 0.000000000000000000 ) ) ;
#16076 = DIRECTION ( 'NONE',  ( 0.000000000000000000, 0.4999999999999990008, -0.8660254037844391517 ) ) ;
#16077 = EDGE_CURVE ( 'NONE', #20036, #9398, #8835, .T. ) ;
#16078 = ADVANCED_FACE ( 'NONE', ( #184 ), #1498, .T. ) ;
#16079 = ORIENTED_EDGE ( 'NONE', *, *, #11023, .F. ) ;
#16080 = CARTESIAN_POINT ( 'NONE',  ( 9.999999999999998224, -51.96384592647165590, -49.83732252579670075 ) ) ;
#16081 = DIRECTION ( 'NONE',  ( 0.000000000000000000, -0.3984010898462296835, -0.9172113015054581542 ) ) ;
#16082 = AXIS2_PLACEMENT_3D ( 'NONE', #8993, #13981, #20318 ) ;
#16083 = VERTEX_POINT ( 'NONE', #14515 ) ;
#16084 = CARTESIAN_POINT ( 'NONE',  ( 0.000000000000000000, 23.08379033237351408, 61.02926039941444003 ) ) ;
#16085 = DIRECTION ( 'NONE',  ( -1.000000000000000000, 0.000000000000000000, 0.000000000000000000 ) ) ;
#16086 = DIRECTION ( 'NONE',  ( -1.836909530733573776E-16, 1.000000000000000000, 0.000000000000000000 ) ) ;
#16087 = ORIENTED_EDGE ( 'NONE', *, *, #1358, .F. ) ;
#16088 = DIRECTION ( 'NONE',  ( -1.000000000000000000, -0.000000000000000000, 0.000000000000000000 ) ) ;
#16089 = CIRCLE ( 'NONE', #17773, 65.24900000006526568 ) ;
#16090 = DIRECTION ( 'NONE',  ( -1.000000000000000000, -0.000000000000000000, 0.000000000000000000 ) ) ;
#16091 = CARTESIAN_POINT ( 'NONE',  ( 6.250000000000203393, 10.82531754730537266, 51.00000000000001421 ) ) ;
#16092 = CARTESIAN_POINT ( 'NONE',  ( -15.25966316918061949, 10.19618095414378800, -8.795356249819690220 ) ) ;
#16093 = EDGE_CURVE ( 'NONE', #18098, #10195, #18749, .T. ) ;
#16094 = ORIENTED_EDGE ( 'NONE', *, *, #5126, .F. ) ;
#16095 = EDGE_CURVE ( 'NONE', #14728, #5755, #14409, .T. ) ;
#16096 = DIRECTION ( 'NONE',  ( 0.000000000000000000, 0.000000000000000000, 1.000000000000000000 ) ) ;
#16097 = CARTESIAN_POINT ( 'NONE',  ( 40.00000000000036948, -40.00000000000055422, -51.99999999999928946 ) ) ;
#16098 = DIRECTION ( 'NONE',  ( -0.000000000000000000, -0.000000000000000000, -1.000000000000000000 ) ) ;
#16099 = CARTESIAN_POINT ( 'NONE',  ( -8.382925368423267187, 12.54593441764186856, -11.96763566848092530 ) ) ;
#16100 = CARTESIAN_POINT ( 'NONE',  ( 11.50000000000001066, -85.00000000000000000, 19.00000000000000000 ) ) ;
#16101 = EDGE_CURVE ( 'NONE', #12626, #2621, #18078, .T. ) ;
#16102 = COLOUR_RGB ( '', 0.09019608, 0.27058824, 0.51372549) ;
#16103 = ORIENTED_EDGE ( 'NONE', *, *, #15149, .F. ) ;
#16104 = DIRECTION ( 'NONE',  ( -1.000000000000000000, 0.000000000000000000, 0.000000000000000000 ) ) ;
#16105 = DIRECTION ( 'NONE',  ( -1.000000000000000000, 0.000000000000000000, -0.000000000000000000 ) ) ;
#16106 = DIRECTION ( 'NONE',  ( 1.000000000000000000, 0.000000000000000000, 0.000000000000000000 ) ) ;
#16107 = ORIENTED_EDGE ( 'NONE', *, *, #12098, .F. ) ;
#16108 = LINE ( 'NONE', #8143, #9896 ) ;
#16109 = ORIENTED_EDGE ( 'NONE', *, *, #19203, .F. ) ;
#16110 = CARTESIAN_POINT ( 'NONE',  ( -25.39999999999999858, 0.000000000000000000, 7.500000000000000000 ) ) ;
#16111 = DIRECTION ( 'NONE',  ( -1.000000000000000000, 0.000000000000000000, 0.000000000000000000 ) ) ;
#16112 = ORIENTED_EDGE ( 'NONE', *, *, #16218, .T. ) ;
#16113 = EDGE_CURVE ( 'NONE', #13788, #9017, #9603, .T. ) ;
#16114 = EDGE_LOOP ( 'NONE', ( #10512, #1697, #16369, #20479 ) ) ;
#16115 = CARTESIAN_POINT ( 'NONE',  ( 48.31551312895897610, -3.761933334864634215, -82.40301848942678475 ) ) ;
#16116 = EDGE_CURVE ( 'NONE', #2965, #16270, #7156, .T. ) ;
#16117 = AXIS2_PLACEMENT_3D ( 'NONE', #9508, #14806, #71 ) ;
#16118 = FILL_AREA_STYLE ('',( #9654 ) ) ;
#16119 = CARTESIAN_POINT ( 'NONE',  ( -30.00000000000000000, -124.9999999999999858, 90.00000000000001421 ) ) ;
#16120 = VECTOR ( 'NONE', #4576, 1000.000000000000000 ) ;
#16121 = EDGE_CURVE ( 'NONE', #12516, #10498, #3668, .T. ) ;
#16122 =( NAMED_UNIT ( * ) SI_UNIT ( $, .STERADIAN. ) SOLID_ANGLE_UNIT ( ) );
#16123 = CARTESIAN_POINT ( 'NONE',  ( -4.248408730893249441, -6.358192987158595599, 19.30354375018031732 ) ) ;
#16124 = CARTESIAN_POINT ( 'NONE',  ( -6.330490858644137298, -9.474249097082495297, 3.184733999713198038 ) ) ;
#16125 = DIRECTION ( 'NONE',  ( 0.000000000000000000, 0.000000000000000000, -1.000000000000000000 ) ) ;
#16126 = DIRECTION ( 'NONE',  ( -1.000000000000000000, 0.000000000000000000, 0.000000000000000000 ) ) ;
#16127 = DIRECTION ( 'NONE',  ( -1.000000000000000000, -0.000000000000000000, -0.000000000000000000 ) ) ;
#16128 = EDGE_LOOP ( 'NONE', ( #9134, #9995, #3099, #18060 ) ) ;
#16129 = CARTESIAN_POINT ( 'NONE',  ( 9.999999999999998224, 64.36139404986010959, -32.27399814043808846 ) ) ;
#16130 = AXIS2_PLACEMENT_3D ( 'NONE', #10294, #4021, #2236 ) ;
#16131 = VERTEX_POINT ( 'NONE', #7054 ) ;
#16132 = CARTESIAN_POINT ( 'NONE',  ( -3.580422614997675002, -17.99999999956958163, 7.109331250180313866 ) ) ;
#16133 = DIRECTION ( 'NONE',  ( -1.000000000000000000, -0.000000000000000000, -0.000000000000000000 ) ) ;
#16134 = ORIENTED_EDGE ( 'NONE', *, *, #15854, .T. ) ;
#16135 = DIRECTION ( 'NONE',  ( -1.000000000000000000, -0.000000000000000000, -0.000000000000000000 ) ) ;
#16136 = CIRCLE ( 'NONE', #225, 4.000000000000000000 ) ;
#16137 = ORIENTED_EDGE ( 'NONE', *, *, #11453, .T. ) ;
#16138 = DIRECTION ( 'NONE',  ( 0.000000000000000000, 0.000000000000000000, 1.000000000000000000 ) ) ;
#16139 = CARTESIAN_POINT ( 'NONE',  ( 34.00864524562752678, -27.73747959566527399, 73.62555811687104779 ) ) ;
#16140 = AXIS2_PLACEMENT_3D ( 'NONE', #1197, #19604, #11457 ) ;
#16141 = VERTEX_POINT ( 'NONE', #16917 ) ;
#16142 = ORIENTED_EDGE ( 'NONE', *, *, #5087, .T. ) ;
#16143 = CARTESIAN_POINT ( 'NONE',  ( 19.99999999999999645, -58.26603306961992246, 42.29739224042451440 ) ) ;
#16144 = AXIS2_PLACEMENT_3D ( 'NONE', #5742, #13597, #20045 ) ;
#16145 = LINE ( 'NONE', #5282, #7523 ) ;
#16146 = CARTESIAN_POINT ( 'NONE',  ( 9.999999999999998224, -0.9548212943370527617, 71.99366858485716136 ) ) ;
#16147 = CIRCLE ( 'NONE', #15123, 72.00000000007199219 ) ;
#16148 = CYLINDRICAL_SURFACE ( 'NONE', #13663, 2.649999999999994582 ) ;
#16149 = ORIENTED_EDGE ( 'NONE', *, *, #13871, .F. ) ;
#16150 = AXIS2_PLACEMENT_3D ( 'NONE', #493, #18284, #18796 ) ;
#16151 = CARTESIAN_POINT ( 'NONE',  ( 2.870125741905211747, -6.929096494179675325, 11.56598750018031296 ) ) ;
#16152 = COLOUR_RGB ( '', 0.08235294, 0.09019608, 0.10196078) ;
#16153 = LINE ( 'NONE', #1647, #10159 ) ;
#16154 = CARTESIAN_POINT ( 'NONE',  ( 0.000000000000000000, 24.01204443665187327, 60.22865198596132785 ) ) ;
#16155 = CARTESIAN_POINT ( 'NONE',  ( 40.00000000000000711, 39.99999999999998579, -120.0000000000000142 ) ) ;
#16156 = ORIENTED_EDGE ( 'NONE', *, *, #18263, .F. ) ;
#16157 = EDGE_CURVE ( 'NONE', #19080, #5222, #19711, .T. ) ;
#16158 = CARTESIAN_POINT ( 'NONE',  ( 18.00000000000000000, -2.163824016901520184E-09, -23.81644999981969235 ) ) ;
#16159 = CARTESIAN_POINT ( 'NONE',  ( 12.72792206288790950, 12.72792205982780089, 20.22582500018031837 ) ) ;
#16160 = CARTESIAN_POINT ( 'NONE',  ( -12.50000000000000533, 0.000000000000000000, 166.0000000000000000 ) ) ;
#16161 = AXIS2_PLACEMENT_3D ( 'NONE', #10713, #17177, #2659 ) ;
#16162 = ORIENTED_EDGE ( 'NONE', *, *, #17550, .F. ) ;
#16163 = FACE_BOUND ( 'NONE', #15101, .T. ) ;
#16164 = VERTEX_POINT ( 'NONE', #2085 ) ;
#16165 = CARTESIAN_POINT ( 'NONE',  ( 11.50000000000000000, 1.408343819019456176E-15, -68.00000000000000000 ) ) ;
#16166 = ORIENTED_EDGE ( 'NONE', *, *, #9875, .F. ) ;
#16167 = AXIS2_PLACEMENT_3D ( 'NONE', #12917, #19268, #11215 ) ;
#16168 = CIRCLE ( 'NONE', #12094, 10.00000000000000178 ) ;
#16169 = CARTESIAN_POINT ( 'NONE',  ( 19.99999999999999645, -20.60847369612940128, -61.90898814327737654 ) ) ;
#16170 = CARTESIAN_POINT ( 'NONE',  ( 19.99999999999999645, -63.48283426024874387, 33.96954156735347397 ) ) ;
#16171 = VECTOR ( 'NONE', #15867, 1000.000000000000000 ) ;
#16172 = CARTESIAN_POINT ( 'NONE',  ( 14.79893867722910450, -2.943691928843438443, -12.24017683115845578 ) ) ;
#16173 = ORIENTED_EDGE ( 'NONE', *, *, #10701, .F. ) ;
#16174 = DIRECTION ( 'NONE',  ( 0.000000000000000000, 0.000000000000000000, -1.000000000000000000 ) ) ;
#16175 = AXIS2_PLACEMENT_3D ( 'NONE', #6921, #13712, #10111 ) ;
#16176 = DIRECTION ( 'NONE',  ( -1.000000000000000000, -0.000000000000000000, -0.000000000000000000 ) ) ;
#16177 = EDGE_LOOP ( 'NONE', ( #9841, #20941, #20562, #15848 ) ) ;
#16178 = DIRECTION ( 'NONE',  ( 0.000000000000000000, 0.000000000000000000, 1.000000000000000000 ) ) ;
#16179 = AXIS2_PLACEMENT_3D ( 'NONE', #10142, #8341, #1781 ) ;
#16180 = ADVANCED_FACE ( 'NONE', ( #13534 ), #18296, .T. ) ;
#16181 = FACE_OUTER_BOUND ( 'NONE', #6490, .T. ) ;
#16182 = DIRECTION ( 'NONE',  ( -1.000000000000000000, 0.000000000000000000, 0.000000000000000000 ) ) ;
#16183 = CARTESIAN_POINT ( 'NONE',  ( 19.99999999999999645, -51.96384592647164880, -49.83732252579670075 ) ) ;
#16184 = EDGE_LOOP ( 'NONE', ( #16538, #20385, #13286, #8633 ) ) ;
#16185 = B_SPLINE_CURVE_WITH_KNOTS ( 'NONE', 3,
 ( #9232, #9848, #4769, #6362, #1808, #14840 ),
 .UNSPECIFIED., .F., .F.,
 ( 4, 2, 4 ),
 ( 0.004120275011746849653, 0.005288420935197133549, 0.006456566858647416578 ),
 .UNSPECIFIED. ) ;
#16186 = CYLINDRICAL_SURFACE ( 'NONE', #9054, 27.60000000002759535 ) ;
#16187 = ORIENTED_EDGE ( 'NONE', *, *, #11676, .F. ) ;
#16188 = EDGE_CURVE ( 'NONE', #4706, #6580, #15316, .T. ) ;
#16189 = CARTESIAN_POINT ( 'NONE',  ( 19.99999999999999645, -10.77748419466653651, -63.93680186330482940 ) ) ;
#16190 = CARTESIAN_POINT ( 'NONE',  ( 2.000000000000027089, 3.464101615137739731, -5.600000000000000533 ) ) ;
#16191 = CARTESIAN_POINT ( 'NONE',  ( -6.360000000000001208, 10.85999999999999943, 0.000000000000000000 ) ) ;
#16192 = ORIENTED_EDGE ( 'NONE', *, *, #11853, .T. ) ;
#16193 = FACE_OUTER_BOUND ( 'NONE', #3234, .T. ) ;
#16194 = DIRECTION ( 'NONE',  ( 0.000000000000000000, 0.000000000000000000, 1.000000000000000000 ) ) ;
#16195 = APPLICATION_PROTOCOL_DEFINITION ( 'draft international standard', 'automotive_design', 1998, #316 ) ;
#16196 = CARTESIAN_POINT ( 'NONE',  ( -12.72792205982780089, 12.72792206288791128, -8.500824999819689864 ) ) ;
#16197 = ORIENTED_EDGE ( 'NONE', *, *, #2752, .T. ) ;
#16198 = LINE ( 'NONE', #8042, #10969 ) ;
#16199 = CARTESIAN_POINT ( 'NONE',  ( 19.99999999999999645, -36.54710069451017063, -54.05313526368150434 ) ) ;
#16200 = CARTESIAN_POINT ( 'NONE',  ( -10.46442989454075168, -10.46442989202483709, -14.61841691848093028 ) ) ;
#16201 = DIRECTION ( 'NONE',  ( 0.000000000000000000, 0.000000000000000000, 1.000000000000000000 ) ) ;
#16202 = ORIENTED_EDGE ( 'NONE', *, *, #4720, .T. ) ;
#16203 = LINE ( 'NONE', #1286, #753 ) ;
#16204 = DIRECTION ( 'NONE',  ( 1.000000000000000000, 0.000000000000000000, 0.000000000000000000 ) ) ;
#16205 = CYLINDRICAL_SURFACE ( 'NONE', #11417, 2.649999999999999467 ) ;
#16206 = ORIENTED_EDGE ( 'NONE', *, *, #1322, .T. ) ;
#16207 = EDGE_CURVE ( 'NONE', #14343, #20337, #13294, .T. ) ;
#16208 = DIRECTION ( 'NONE',  ( -1.000000000000000000, -0.000000000000000000, -0.000000000000000000 ) ) ;
#16209 = ORIENTED_EDGE ( 'NONE', *, *, #19310, .F. ) ;
#16210 = CARTESIAN_POINT ( 'NONE',  ( 44.77210880146824223, -9.201386547187325959, -84.14302149088062777 ) ) ;
#16211 = CARTESIAN_POINT ( 'NONE',  ( 16.62983158603121936, 6.888301780572501976, 20.81488750018031197 ) ) ;
#16212 = EDGE_CURVE ( 'NONE', #20215, #2640, #816, .T. ) ;
#16213 = VERTEX_POINT ( 'NONE', #10561 ) ;
#16214 = ORIENTED_EDGE ( 'NONE', *, *, #10275, .T. ) ;
#16215 = DIRECTION ( 'NONE',  ( 0.000000000000000000, 0.000000000000000000, 1.000000000000000000 ) ) ;
#16216 = EDGE_CURVE ( 'NONE', #5396, #14177, #2189, .T. ) ;
#16217 = CYLINDRICAL_SURFACE ( 'NONE', #15788, 5.000000000000004441 ) ;
#16218 = EDGE_CURVE ( 'NONE', #14158, #14374, #10587, .T. ) ;
#16219 = CIRCLE ( 'NONE', #5369, 16.99999999999995026 ) ;
#16220 = DIRECTION ( 'NONE',  ( -1.000000000000000000, 0.000000000000000000, 0.000000000000000000 ) ) ;
#16221 = PRODUCT_RELATED_PRODUCT_CATEGORY ( 'part', '', ( #13917 ) ) ;
#16222 = FACE_OUTER_BOUND ( 'NONE', #4375, .T. ) ;
#16223 = CARTESIAN_POINT ( 'NONE',  ( -5.303300859536636658, -5.303300858261589035, 10.17307500018031519 ) ) ;
#16224 = CARTESIAN_POINT ( 'NONE',  ( 2.222972771497739419, 11.17563879704981922, -2.116828500286803028 ) ) ;
#16225 = CARTESIAN_POINT ( 'NONE',  ( 19.99999999999999645, -53.26727847779570624, 48.44168704307610795 ) ) ;
#16226 = DIRECTION ( 'NONE',  ( 1.000000000000000000, -0.000000000000000000, -0.000000000000000000 ) ) ;
#16227 = ADVANCED_FACE ( 'NONE', ( #18516 ), #8646, .F. ) ;
#16228 = ORIENTED_EDGE ( 'NONE', *, *, #7871, .T. ) ;
#16229 = CARTESIAN_POINT ( 'NONE',  ( -10.00000000000000000, 0.000000000000000000, 0.000000000000000000 ) ) ;
#16230 = CARTESIAN_POINT ( 'NONE',  ( -18.00000000043041126, -3.580422610670022543, 8.876518750180315109 ) ) ;
#16231 = FACE_OUTER_BOUND ( 'NONE', #19940, .T. ) ;
#16232 = ORIENTED_EDGE ( 'NONE', *, *, #15962, .F. ) ;
#16233 = EDGE_CURVE ( 'NONE', #20839, #9747, #6519, .T. ) ;
#16234 = DIRECTION ( 'NONE',  ( -1.000000000000000000, -0.000000000000000000, -0.000000000000000000 ) ) ;
#16235 = VERTEX_POINT ( 'NONE', #18204 ) ;
#16236 = PLANE ( 'NONE',  #14920 ) ;
#16237 = DIRECTION ( 'NONE',  ( 0.000000000000000000, -0.2697967711570115612, -0.9629172873478027972 ) ) ;
#16238 = EDGE_CURVE ( 'NONE', #701, #1492, #18026, .T. ) ;
#16239 = ORIENTED_EDGE ( 'NONE', *, *, #18404, .F. ) ;
#16240 = ORIENTED_EDGE ( 'NONE', *, *, #17268, .F. ) ;
#16241 = FACE_OUTER_BOUND ( 'NONE', #4339, .T. ) ;
#16242 = EDGE_CURVE ( 'NONE', #1429, #8808, #4140, .T. ) ;
#16243 = DIRECTION ( 'NONE',  ( 1.000000000000000000, -0.000000000000000000, -0.000000000000000000 ) ) ;
#16244 = FACE_OUTER_BOUND ( 'NONE', #13810, .T. ) ;
#16245 = ORIENTED_EDGE ( 'NONE', *, *, #288, .F. ) ;
#16246 = AXIS2_PLACEMENT_3D ( 'NONE', #20807, #10961, #15933 ) ;
#16247 = CARTESIAN_POINT ( 'NONE',  ( 1.491842756249028845, 7.499999999820661678, 7.737081250180311898 ) ) ;
#16248 = DIRECTION ( 'NONE',  ( 1.000000000000000000, 0.000000000000000000, 0.000000000000000000 ) ) ;
#16249 = CARTESIAN_POINT ( 'NONE',  ( 54.64999999999999858, -99.99999999999998579, 0.000000000000000000 ) ) ;
#16250 = DIRECTION ( 'NONE',  ( 0.000000000000000000, 0.000000000000000000, 1.000000000000000000 ) ) ;
#16251 = EDGE_CURVE ( 'NONE', #14272, #11488, #1131, .T. ) ;
#16252 = EDGE_LOOP ( 'NONE', ( #20746, #3035, #16385, #19205, #13036, #3433, #13480, #2434, #19903 ) ) ;
#16253 = CARTESIAN_POINT ( 'NONE',  ( 85.00002539999999840, 9.184850993605147944E-16, -7.500000000000000000 ) ) ;
#16254 = CARTESIAN_POINT ( 'NONE',  ( -4.000000000000000000, 2.309401076758496263, -0.3572655899081631503 ) ) ;
#16255 = CARTESIAN_POINT ( 'NONE',  ( 0.000000000000000000, 0.000000000000000000, -40.00000000000000000 ) ) ;
#16256 = ORIENTED_EDGE ( 'NONE', *, *, #14598, .F. ) ;
#16257 = DIRECTION ( 'NONE',  ( 1.000000000000000000, 0.000000000000000000, 0.000000000000000000 ) ) ;
#16258 = VERTEX_POINT ( 'NONE', #8754 ) ;
#16259 = CYLINDRICAL_SURFACE ( 'NONE', #1036, 27.60000000002759890 ) ;
#16260 = EDGE_LOOP ( 'NONE', ( #2195, #10475, #4255, #12095 ) ) ;
#16261 = AXIS2_PLACEMENT_3D ( 'NONE', #19014, #2797, #4489 ) ;
#16262 = CARTESIAN_POINT ( 'NONE',  ( 19.99999999999999645, -6.872116855663586321, 64.47358224882414390 ) ) ;
#16263 = EDGE_CURVE ( 'NONE', #7264, #18514, #8218, .T. ) ;
#16264 = DIRECTION ( 'NONE',  ( 0.000000000000000000, -0.000000000000000000, 1.000000000000000000 ) ) ;
#16265 = AXIS2_PLACEMENT_3D ( 'NONE', #9031, #15492, #8915 ) ;
#16266 = CARTESIAN_POINT ( 'NONE',  ( -2.222972768810837607, 11.17563879758428769, 23.26682850064743491 ) ) ;
#16267 = ORIENTED_EDGE ( 'NONE', *, *, #17932, .T. ) ;
#16268 = CARTESIAN_POINT ( 'NONE',  ( -2.339468227445729021, -3.268109542640674547, -5.599999999999982769 ) ) ;
#16269 = DIRECTION ( 'NONE',  ( -1.000000000000000000, -0.000000000000000000, -0.000000000000000000 ) ) ;
#16270 = VERTEX_POINT ( 'NONE', #5676 ) ;
#16271 = DIRECTION ( 'NONE',  ( 0.000000000000000000, 0.3984010898462422845, -0.9172113015054527141 ) ) ;
#16272 = DIRECTION ( 'NONE',  ( -1.000000000000000000, -0.000000000000000000, -0.000000000000000000 ) ) ;
#16273 = DIRECTION ( 'NONE',  ( -0.000000000000000000, -0.000000000000000000, 1.000000000000000000 ) ) ;
#16274 = DIRECTION ( 'NONE',  ( 0.000000000000000000, 0.000000000000000000, -1.000000000000000000 ) ) ;
#16275 = ORIENTED_EDGE ( 'NONE', *, *, #19216, .T. ) ;
#16276 = CARTESIAN_POINT ( 'NONE',  ( -2.000000000000022649, -3.464101615137742396, 0.000000000000000000 ) ) ;
#16277 = AXIS2_PLACEMENT_3D ( 'NONE', #13705, #18584, #9044 ) ;
#16278 = ORIENTED_EDGE ( 'NONE', *, *, #5598, .T. ) ;
#16279 = CARTESIAN_POINT ( 'NONE',  ( 24.99999999999999645, -99.99999999999998579, -52.00000000000000000 ) ) ;
#16280 = LINE ( 'NONE', #3448, #20494 ) ;
#16281 = CARTESIAN_POINT ( 'NONE',  ( 17.99999999956957808, -3.580422614997675446, -25.42651874981969584 ) ) ;
#16282 = VERTEX_POINT ( 'NONE', #19782 ) ;
#16283 = CARTESIAN_POINT ( 'NONE',  ( 6.358192987158596488, -4.248408730893249441, -11.32770624981968588 ) ) ;
#16284 = EDGE_CURVE ( 'NONE', #15627, #12643, #17025, .T. ) ;
#16285 = CARTESIAN_POINT ( 'NONE',  ( 19.99999999999999645, 0.000000000000000000, 0.000000000000000000 ) ) ;
#16286 = DIRECTION ( 'NONE',  ( 6.123233995736668661E-17, -1.060575238724912831E-16, -1.000000000000000000 ) ) ;
#16287 = CARTESIAN_POINT ( 'NONE',  ( 3.580422614997669228, 17.99999999956958874, -16.45316874981969590 ) ) ;
#16289 = ORIENTED_EDGE ( 'NONE', *, *, #16077, .T. ) ;
#16288 = AXIS2_PLACEMENT_3D ( 'NONE', #4711, #4807, #16051 ) ;
#16290 = CARTESIAN_POINT ( 'NONE',  ( -6.358192987158592047, 4.248408730893246776, 5.969893750180308878 ) ) ;
#16291 = AXIS2_PLACEMENT_3D ( 'NONE', #10178, #12092, #5302 ) ;
#16292 = DIRECTION ( 'NONE',  ( 0.000000000000000000, 0.000000000000000000, 1.000000000000000000 ) ) ;
#16293 = CARTESIAN_POINT ( 'NONE',  ( -2.943691928843435779, -14.79893867722909917, -6.077010668480928857 ) ) ;
#16294 = CARTESIAN_POINT ( 'NONE',  ( 2.500000000000000000, 2.357898499370433054, -1.951563910473907981E-15 ) ) ;
#16295 = CIRCLE ( 'NONE', #3098, 65.24900000006525147 ) ;
#16296 = ORIENTED_EDGE ( 'NONE', *, *, #5685, .F. ) ;
#16297 = CARTESIAN_POINT ( 'NONE',  ( 0.000000000000000000, -54.08351995568730786, 35.76369202524482915 ) ) ;
#16298 = CARTESIAN_POINT ( 'NONE',  ( 8.900000000000046541, 10.82531754730546147, 43.00000000000000000 ) ) ;
#16299 = DIRECTION ( 'NONE',  ( 0.000000000000000000, 0.000000000000000000, 1.000000000000000000 ) ) ;
#16300 = ORIENTED_EDGE ( 'NONE', *, *, #4194, .F. ) ;
#16301 = AXIS2_PLACEMENT_3D ( 'NONE', #20073, #10447, #7462 ) ;
#16302 = DIRECTION ( 'NONE',  ( -1.000000000000000000, -0.000000000000000000, 0.000000000000000000 ) ) ;
#16303 = CIRCLE ( 'NONE', #4459, 2.099999999999990763 ) ;
#16304 = ORIENTED_EDGE ( 'NONE', *, *, #1831, .F. ) ;
#16305 = CARTESIAN_POINT ( 'NONE',  ( -62.49999999999999289, -40.00000000000000000, 5.000000000000000000 ) ) ;
#16306 = DIRECTION ( 'NONE',  ( 1.000000000000000000, 0.000000000000000000, 0.000000000000000000 ) ) ;
#16307 = ORIENTED_EDGE ( 'NONE', *, *, #6369, .F. ) ;
#16308 = CIRCLE ( 'NONE', #15629, 75.00000000000001421 ) ;
#16309 = VERTEX_POINT ( 'NONE', #9289 ) ;
#16310 = CARTESIAN_POINT ( 'NONE',  ( 48.36605527348424971, -3.740379660666403261, 82.39768715423042522 ) ) ;
#16311 = LINE ( 'NONE', #14934, #16467 ) ;
#16312 = CIRCLE ( 'NONE', #19354, 7.567219999999999835 ) ;
#16313 = LINE ( 'NONE', #4768, #12311 ) ;
#16314 = CARTESIAN_POINT ( 'NONE',  ( 7.499999999820668783, -1.491842756249033508, 16.35823125018031376 ) ) ;
#16315 = VECTOR ( 'NONE', #8992, 1000.000000000000000 ) ;
#16316 = EDGE_CURVE ( 'NONE', #19366, #10081, #17011, .T. ) ;
#16317 = AXIS2_PLACEMENT_3D ( 'NONE', #2121, #15054, #321 ) ;
#16318 = CARTESIAN_POINT ( 'NONE',  ( -11.17563879731704723, 1.343452237168308679E-09, -4.767609750286803560 ) ) ;
#16319 = CIRCLE ( 'NONE', #1122, 4.000000000000000000 ) ;
#16320 = ADVANCED_FACE ( 'NONE', ( #14179 ), #1462, .T. ) ;
#16321 = AXIS2_PLACEMENT_3D ( 'NONE', #16537, #8471, #15059 ) ;
#16322 = DIRECTION ( 'NONE',  ( -1.000000000000000000, -0.000000000000000000, -0.000000000000000000 ) ) ;
#16323 = DIRECTION ( 'NONE',  ( 0.000000000000000000, 0.000000000000000000, 1.000000000000000000 ) ) ;
#16324 = VERTEX_POINT ( 'NONE', #11095 ) ;
#16325 = DIRECTION ( 'NONE',  ( -1.000000000000000000, -0.000000000000000000, -0.000000000000000000 ) ) ;
#16326 = CARTESIAN_POINT ( 'NONE',  ( 18.00000000000000000, -2.163824016901520184E-09, 23.30855000018031475 ) ) ;
#16327 = CARTESIAN_POINT ( 'NONE',  ( 19.99999999999999645, -23.08379033237394395, 61.02926039941428371 ) ) ;
#16328 = ADVANCED_FACE ( 'NONE', ( #18835 ), #2513, .T. ) ;
#16329 = ORIENTED_EDGE ( 'NONE', *, *, #18044, .T. ) ;
#16330 = CARTESIAN_POINT ( 'NONE',  ( 3.599999999999913936, -10.82531754730554496, 126.0000000000000000 ) ) ;
#16331 = ORIENTED_EDGE ( 'NONE', *, *, #4033, .T. ) ;
#16332 = LINE ( 'NONE', #14552, #5768 ) ;
#16333 = CARTESIAN_POINT ( 'NONE',  ( 3.345653888883671545, -2.687187980154741140, -5.460849780464844372 ) ) ;
#16334 = VERTEX_POINT ( 'NONE', #9083 ) ;
#16335 = ORIENTED_EDGE ( 'NONE', *, *, #19593, .F. ) ;
#16336 = FACE_OUTER_BOUND ( 'NONE', #5790, .T. ) ;
#16337 = AXIS2_PLACEMENT_3D ( 'NONE', #5762, #2383, #5665 ) ;
#16338 = VECTOR ( 'NONE', #8762, 1000.000000000000000 ) ;
#16339 = CARTESIAN_POINT ( 'NONE',  ( 3.999999999999990674, -2.309401076758548221, -0.3572655899081733644 ) ) ;
#16340 = EDGE_CURVE ( 'NONE', #17345, #2098, #2451, .T. ) ;
#16341 = DIRECTION ( 'NONE',  ( 0.000000000000000000, -0.000000000000000000, 1.000000000000000000 ) ) ;
#16342 = CIRCLE ( 'NONE', #12640, 27.60000000002759890 ) ;
#16343 = VERTEX_POINT ( 'NONE', #12573 ) ;
#16344 = EDGE_CURVE ( 'NONE', #10009, #9276, #10982, .T. ) ;
#16345 = CARTESIAN_POINT ( 'NONE',  ( -6.358192988180014993, -4.248408729364575365, 13.62770625018031367 ) ) ;
#16346 = EDGE_CURVE ( 'NONE', #1099, #20364, #12369, .T. ) ;
#16347 = CARTESIAN_POINT ( 'NONE',  ( 30.00000000000000000, -39.99999999999999289, 54.09999999999998721 ) ) ;
#16348 = AXIS2_PLACEMENT_3D ( 'NONE', #18269, #15094, #7448 ) ;
#16349 = CARTESIAN_POINT ( 'NONE',  ( -62.49999999999999289, -30.00000000000000000, 5.000000000000000000 ) ) ;
#16350 = DIRECTION ( 'NONE',  ( -0.000000000000000000, 0.000000000000000000, -1.000000000000000000 ) ) ;
#16351 = VERTEX_POINT ( 'NONE', #4200 ) ;
#16352 = DIRECTION ( 'NONE',  ( 0.000000000000000000, 0.000000000000000000, -1.000000000000000000 ) ) ;
#16353 = ORIENTED_EDGE ( 'NONE', *, *, #4677, .T. ) ;
#16354 = EDGE_CURVE ( 'NONE', #17620, #6859, #5838, .T. ) ;
#16355 = CARTESIAN_POINT ( 'NONE',  ( 12.72792205982779734, -12.72792206288791128, 13.15707500018031517 ) ) ;
#16356 = DIRECTION ( 'NONE',  ( -0.000000000000000000, -0.000000000000000000, 1.000000000000000000 ) ) ;
#16357 = EDGE_LOOP ( 'NONE', ( #7365, #7132, #494, #5165 ) ) ;
#16358 = DIRECTION ( 'NONE',  ( -0.000000000000000000, -0.000000000000000000, 1.000000000000000000 ) ) ;
#16359 = VERTEX_POINT ( 'NONE', #12691 ) ;
#16360 = CARTESIAN_POINT ( 'NONE',  ( 50.00000000000000000, 230.0000000000000000, 0.000000000000000000 ) ) ;
#16361 = EDGE_LOOP ( 'NONE', ( #9600, #11503, #4207, #8032 ) ) ;
#16362 = ADVANCED_FACE ( 'NONE', ( #6001 ), #10677, .F. ) ;
#16363 = DIRECTION ( 'NONE',  ( -1.000000000000000000, 0.000000000000000000, 0.000000000000000000 ) ) ;
#16364 = AXIS2_PLACEMENT_3D ( 'NONE', #7557, #12773, #4596 ) ;
#16365 = AXIS2_PLACEMENT_3D ( 'NONE', #17, #8081, #3093 ) ;
#16366 = EDGE_CURVE ( 'NONE', #1411, #19744, #9236, .T. ) ;
#16367 = DIRECTION ( 'NONE',  ( 1.000000000000000000, 0.000000000000000000, 0.000000000000000000 ) ) ;
#16368 = CARTESIAN_POINT ( 'NONE',  ( -13.67243654642775574, 5.663308650141533285, -16.65814558115846111 ) ) ;
#16369 = ORIENTED_EDGE ( 'NONE', *, *, #19092, .T. ) ;
#16370 = SURFACE_SIDE_STYLE ('',( #11398 ) ) ;
#16371 = ADVANCED_FACE ( 'NONE', ( #9179 ), #17346, .T. ) ;
#16372 = DIRECTION ( 'NONE',  ( 0.000000000000000000, 0.000000000000000000, 1.000000000000000000 ) ) ;
#16373 = EDGE_LOOP ( 'NONE', ( #14724, #17207, #20830 ) ) ;
#16374 = VECTOR ( 'NONE', #8917, 1000.000000000000000 ) ;
#16375 = CARTESIAN_POINT ( 'NONE',  ( 5.303300858261583706, -5.303300859536632217, -26.72307499981969414 ) ) ;
#16376 = AXIS2_PLACEMENT_3D ( 'NONE', #14605, #8340, #82 ) ;
#16377 = ORIENTED_EDGE ( 'NONE', *, *, #4562, .F. ) ;
#16378 = CARTESIAN_POINT ( 'NONE',  ( 0.000000000000000000, 1.178949249685213863, -2.042000000000001148 ) ) ;
#16379 = DIRECTION ( 'NONE',  ( 1.000000000000000000, 0.000000000000000000, -0.000000000000000000 ) ) ;
#16380 = CYLINDRICAL_SURFACE ( 'NONE', #1244, 72.00000000007199219 ) ;
#16381 = VECTOR ( 'NONE', #2343, 1000.000000000000000 ) ;
#16382 = ORIENTED_EDGE ( 'NONE', *, *, #18493, .T. ) ;
#16383 = AXIS2_PLACEMENT_3D ( 'NONE', #20702, #11174, #18818 ) ;
#16384 = PLANE ( 'NONE',  #929 ) ;
#16385 = ORIENTED_EDGE ( 'NONE', *, *, #17940, .T. ) ;
#16386 = DIRECTION ( 'NONE',  ( 1.000000000000000000, 0.000000000000000000, 0.000000000000000000 ) ) ;
#16387 = AXIS2_PLACEMENT_3D ( 'NONE', #1002, #15194, #782 ) ;
#16388 = ORIENTED_EDGE ( 'NONE', *, *, #17020, .T. ) ;
#16389 = CARTESIAN_POINT ( 'NONE',  ( 7.500000000000009770, -8.788009009181406898E-15, -12.21129999999768501 ) ) ;
#16390 = LINE ( 'NONE', #77, #5154 ) ;
#16391 = CARTESIAN_POINT ( 'NONE',  ( 6.888301784570730391, 16.62983158437510411, -6.733637499819693062 ) ) ;
#16392 = VERTEX_POINT ( 'NONE', #15641 ) ;
#16393 = CIRCLE ( 'NONE', #17431, 65.24900000006525147 ) ;
#16394 = DIRECTION ( 'NONE',  ( -1.000000000000000000, -0.000000000000000000, -0.000000000000000000 ) ) ;
#16395 = CARTESIAN_POINT ( 'NONE',  ( 3.600000000000066702, 10.82531754730546147, 46.00000000000000711 ) ) ;
#16396 = CARTESIAN_POINT ( 'NONE',  ( -5.663308650141535949, -13.67243654642774686, 3.642520581519076650 ) ) ;
#16397 = DIRECTION ( 'NONE',  ( -0.000000000000000000, -0.000000000000000000, 1.000000000000000000 ) ) ;
#16398 = AXIS2_PLACEMENT_3D ( 'NONE', #5919, #11114, #8036 ) ;
#16399 = EDGE_CURVE ( 'NONE', #18355, #17230, #4515, .T. ) ;
#16400 = ORIENTED_EDGE ( 'NONE', *, *, #6078, .F. ) ;
#16401 = EDGE_CURVE ( 'NONE', #4706, #3596, #15434, .T. ) ;
#16402 = DIRECTION ( 'NONE',  ( 0.000000000000000000, 0.000000000000000000, 1.000000000000000000 ) ) ;
#16403 = DIRECTION ( 'NONE',  ( 0.000000000000000000, 0.5195839500354344498, -0.8544194045464880150 ) ) ;
#16404 = CARTESIAN_POINT ( 'NONE',  ( 11.50000000000001066, -85.00000000000000000, 5.000000000000000000 ) ) ;
#16405 = ORIENTED_EDGE ( 'NONE', *, *, #16354, .T. ) ;
#16406 = DIRECTION ( 'NONE',  ( 0.000000000000000000, 0.000000000000000000, 1.000000000000000000 ) ) ;
#16407 = ORIENTED_EDGE ( 'NONE', *, *, #10651, .T. ) ;
#16408 = CIRCLE ( 'NONE', #16740, 72.00000000007199219 ) ;
#16409 = DIRECTION ( 'NONE',  ( 0.000000000000000000, 0.000000000000000000, 1.000000000000000000 ) ) ;
#16410 = DIRECTION ( 'NONE',  ( 1.000000000000000000, -0.000000000000000000, -0.000000000000000000 ) ) ;
#16411 = ORIENTED_EDGE ( 'NONE', *, *, #8097, .T. ) ;
#16412 = ORIENTED_EDGE ( 'NONE', *, *, #20714, .T. ) ;
#16413 = CARTESIAN_POINT ( 'NONE',  ( -6.999999999999995559, 4.546351088565595293E-15, 0.000000000000000000 ) ) ;
#16414 = DIRECTION ( 'NONE',  ( -0.000000000000000000, 0.000000000000000000, -1.000000000000000000 ) ) ;
#16415 = SURFACE_STYLE_FILL_AREA ( #9845 ) ;
#16416 = PRODUCT_DEFINITION_FORMATION_WITH_SPECIFIED_SOURCE ( 'ANY', '', #7298, .NOT_KNOWN. ) ;
#16417 = CARTESIAN_POINT ( 'NONE',  ( -12.50000000000000533, 0.000000000000000000, 46.00000000000000711 ) ) ;
#16418 = CARTESIAN_POINT ( 'NONE',  ( 6.929096494179683319, 2.870125741905213079, 24.89963750018031519 ) ) ;
#16419 = EDGE_CURVE ( 'NONE', #4388, #8586, #15317, .T. ) ;
#16420 = CARTESIAN_POINT ( 'NONE',  ( -9.474249098604506258, -6.330490856366290053, -5.651203500286803738 ) ) ;
#16421 = FACE_OUTER_BOUND ( 'NONE', #13233, .T. ) ;
#16422 = CARTESIAN_POINT ( 'NONE',  ( 19.99999999999999645, 0.000000000000000000, 0.000000000000000000 ) ) ;
#16423 = VERTEX_POINT ( 'NONE', #4407 ) ;
#16424 = EDGE_CURVE ( 'NONE', #11920, #13947, #16673, .T. ) ;
#16425 = CARTESIAN_POINT ( 'NONE',  ( 19.99999999999999645, 19.38316218894212639, 61.87375713200996330 ) ) ;
#16426 = CARTESIAN_POINT ( 'NONE',  ( -3.580422610670018546, 18.00000000043041126, 20.65776875018031333 ) ) ;
#16427 = FACE_OUTER_BOUND ( 'NONE', #5633, .T. ) ;
#16428 = ORIENTED_EDGE ( 'NONE', *, *, #16316, .T. ) ;
#16429 = CARTESIAN_POINT ( 'NONE',  ( 0.000000000000000000, -2.357898499370432610, 3.252606517456513302E-15 ) ) ;
#16430 = ORIENTED_EDGE ( 'NONE', *, *, #4702, .T. ) ;
#16431 = DIRECTION ( 'NONE',  ( 0.000000000000000000, 0.000000000000000000, 1.000000000000000000 ) ) ;
#16432 = CARTESIAN_POINT ( 'NONE',  ( 9.999999999999998224, 58.26603306962022089, -42.29739224042413070 ) ) ;
#16433 = CIRCLE ( 'NONE', #17464, 27.60000000002759890 ) ;
#16434 = ORIENTED_EDGE ( 'NONE', *, *, #4406, .F. ) ;
#16435 =( REPRESENTATION_RELATIONSHIP ('NONE','NONE', #13739, #12383 ) REPRESENTATION_RELATIONSHIP_WITH_TRANSFORMATION ( #17453 )SHAPE_REPRESENTATION_RELATIONSHIP( ) );
#16436 = ORIENTED_EDGE ( 'NONE', *, *, #4320, .F. ) ;
#16437 = CARTESIAN_POINT ( 'NONE',  ( 11.50000000000001066, -85.00000000000000000, 19.00000000000000000 ) ) ;
#16438 = ADVANCED_FACE ( 'NONE', ( #5777 ), #20410, .T. ) ;
#16439 = CIRCLE ( 'NONE', #5596, 11.50000000000000000 ) ;
#16440 = CARTESIAN_POINT ( 'NONE',  ( 19.99999999999999645, 63.85430960833490843, -11.25592921604860663 ) ) ;
#16441 = CARTESIAN_POINT ( 'NONE',  ( 19.99999999999999645, 58.44960523466241398, -28.06621538408611016 ) ) ;
#16442 = EDGE_CURVE ( 'NONE', #7461, #4444, #7926, .T. ) ;
#16443 = EDGE_CURVE ( 'NONE', #3991, #4894, #14322, .T. ) ;
#16444 = ORIENTED_EDGE ( 'NONE', *, *, #381, .T. ) ;
#16445 = MECHANICAL_DESIGN_GEOMETRIC_PRESENTATION_REPRESENTATION (  '', ( #10021 ), #12701 ) ;
#16446 = CARTESIAN_POINT ( 'NONE',  ( -2.870125741905209971, 6.929096494179676213, 16.27848750018031154 ) ) ;
#16447 = AXIS2_PLACEMENT_3D ( 'NONE', #4592, #1418, #11057 ) ;
#16448 = CYLINDRICAL_SURFACE ( 'NONE', #14578, 27.60000000002760245 ) ;
#16449 = CARTESIAN_POINT ( 'NONE',  ( 17.00000000000000000, 0.000000000000000000, 0.000000000000000000 ) ) ;
#16450 = CYLINDRICAL_SURFACE ( 'NONE', #9291, 2.649999999999993694 ) ;
#16451 = LINE ( 'NONE', #8292, #10620 ) ;
#16452 = CIRCLE ( 'NONE', #8328, 27.60000000002759535 ) ;
#16453 = AXIS2_PLACEMENT_3D ( 'NONE', #20723, #1567, #8021 ) ;
#16454 = ORIENTED_EDGE ( 'NONE', *, *, #16985, .F. ) ;
#16455 = DIRECTION ( 'NONE',  ( 1.000000000000000000, 1.836909530733573776E-16, 0.000000000000000000 ) ) ;
#16456 = ORIENTED_EDGE ( 'NONE', *, *, #4230, .T. ) ;
#16457 = CARTESIAN_POINT ( 'NONE',  ( 19.99999999999999645, 0.000000000000000000, 0.000000000000000000 ) ) ;
#16458 = DIRECTION ( 'NONE',  ( -1.000000000000000000, -0.000000000000000000, 0.000000000000000000 ) ) ;
#16459 = ORIENTED_EDGE ( 'NONE', *, *, #1243, .T. ) ;
#16460 = DIRECTION ( 'NONE',  ( 1.000000000000000000, 1.836909530733573776E-16, 0.000000000000000000 ) ) ;
#16461 = VERTEX_POINT ( 'NONE', #8211 ) ;
#16462 = DIRECTION ( 'NONE',  ( 0.000000000000000000, 0.000000000000000000, -1.000000000000000000 ) ) ;
#16463 = DIRECTION ( 'NONE',  ( 0.000000000000000000, 0.000000000000000000, 1.000000000000000000 ) ) ;
#16464 = CIRCLE ( 'NONE', #6634, 27.60000000002760245 ) ;
#16465 = VERTEX_POINT ( 'NONE', #12802 ) ;
#16466 = EDGE_CURVE ( 'NONE', #9191, #2016, #12334, .T. ) ;
#16467 = VECTOR ( 'NONE', #17919, 1000.000000000000000 ) ;
#16468 = AXIS2_PLACEMENT_3D ( 'NONE', #17604, #10822, #5940 ) ;
#16469 = EDGE_CURVE ( 'NONE', #6600, #14728, #15953, .T. ) ;
#16470 = CARTESIAN_POINT ( 'NONE',  ( 5.303300859536631329, 5.303300858261585482, -10.22932499981969379 ) ) ;
#16471 = SURFACE_SIDE_STYLE ('',( #17583 ) ) ;
#16472 = CIRCLE ( 'NONE', #2591, 18.00000000000000000 ) ;
#16473 = MECHANICAL_DESIGN_GEOMETRIC_PRESENTATION_REPRESENTATION (  '', ( #1642 ), #10046 ) ;
#16474 = EDGE_CURVE ( 'NONE', #1539, #4998, #16342, .T. ) ;
#16475 = CARTESIAN_POINT ( 'NONE',  ( 17.00000000000000000, 2.789133085058097101E-16, -2.055000000000000160 ) ) ;
#16476 = ADVANCED_FACE ( 'NONE', ( #4828, #17769 ), #11294, .T. ) ;
#16477 = CARTESIAN_POINT ( 'NONE',  ( -4.276731815070949239, -10.32494394706616347, 10.01292225064742958 ) ) ;
#16478 = PRODUCT_RELATED_PRODUCT_CATEGORY ( 'part', '', ( #8811 ) ) ;
#16479 = ORIENTED_EDGE ( 'NONE', *, *, #16121, .T. ) ;
#16480 = CARTESIAN_POINT ( 'NONE',  ( -49.35000000000000142, -39.99999999999999289, 0.000000000000000000 ) ) ;
#16481 = DIRECTION ( 'NONE',  ( -1.000000000000000000, 0.000000000000000000, 0.000000000000000000 ) ) ;
#16482 = VERTEX_POINT ( 'NONE', #8113 ) ;
#16483 = CARTESIAN_POINT ( 'NONE',  ( -12.50000000000000533, 0.000000000000000000, 46.00000000000000711 ) ) ;
#16484 = ORIENTED_EDGE ( 'NONE', *, *, #1614, .F. ) ;
#16485 = CIRCLE ( 'NONE', #8700, 54.99999999999999289 ) ;
#16486 = CARTESIAN_POINT ( 'NONE',  ( 10.19618095414378800, 15.25966316918061416, 21.83589375018031475 ) ) ;
#16487 = CARTESIAN_POINT ( 'NONE',  ( 9.999999999999998224, 20.34307325858883431, -69.06634035770285607 ) ) ;
#16488 = CARTESIAN_POINT ( 'NONE',  ( 0.000000000000000000, -1.178949249685213863, 2.042000000000002924 ) ) ;
#16489 = ADVANCED_FACE ( 'NONE', ( #9707 ), #3237, .T. ) ;
#16490 = EDGE_CURVE ( 'NONE', #8932, #10942, #20050, .T. ) ;
#16491 = CIRCLE ( 'NONE', #18862, 80.00000000000000000 ) ;
#16492 = ORIENTED_EDGE ( 'NONE', *, *, #15320, .T. ) ;
#16493 = LINE ( 'NONE', #14898, #10754 ) ;
#16494 = ORIENTED_EDGE ( 'NONE', *, *, #9973, .T. ) ;
#16495 = DIRECTION ( 'NONE',  ( 0.000000000000000000, 0.8878852184023763305, -0.4600650377311499284 ) ) ;
#16496 = CARTESIAN_POINT ( 'NONE',  ( 6.358192987158596488, -4.248408730893249441, -20.75270624981968837 ) ) ;
#16497 = EDGE_CURVE ( 'NONE', #7112, #17615, #14585, .T. ) ;
#16498 = AXIS2_PLACEMENT_3D ( 'NONE', #12182, #12293, #1180 ) ;
#16499 = VERTEX_POINT ( 'NONE', #6512 ) ;
#16500 = DIRECTION ( 'NONE',  ( 1.000000000000000000, 0.000000000000000000, 0.000000000000000000 ) ) ;
#16501 = ADVANCED_BREP_SHAPE_REPRESENTATION ( '', ( #17543, #12461 ), #19129 ) ;
#16502 = CIRCLE ( 'NONE', #15152, 2.649999999999993694 ) ;
#16503 = DIRECTION ( 'NONE',  ( -1.000000000000000000, -0.000000000000000000, -0.000000000000000000 ) ) ;
#16504 = PRODUCT_CONTEXT ( 'NONE', #10067, 'mechanical' ) ;
#16505 = CARTESIAN_POINT ( 'NONE',  ( -14.79893867722910628, 2.943691928843437111, 11.32232316884154777 ) ) ;
#16507 = ORIENTED_EDGE ( 'NONE', *, *, #5420, .F. ) ;
#16506 = AXIS2_PLACEMENT_3D ( 'NONE', #14516, #9315, #7730 ) ;
#16508 = CARTESIAN_POINT ( 'NONE',  ( -52.00000000000000000, -39.99999999999999289, 5.000000000000000000 ) ) ;
#16509 = ORIENTED_EDGE ( 'NONE', *, *, #15116, .T. ) ;
#16510 = CARTESIAN_POINT ( 'NONE',  ( 12.54593441764186679, 8.382925368423272516, -19.03638566848093205 ) ) ;
#16511 = CARTESIAN_POINT ( 'NONE',  ( 8.899999999999895550, -10.82531754730554496, 46.00000000000000711 ) ) ;
#16512 = ORIENTED_EDGE ( 'NONE', *, *, #10103, .F. ) ;
#16513 = CARTESIAN_POINT ( 'NONE',  ( 19.99999999999999645, 0.000000000000000000, 0.000000000000000000 ) ) ;
#16514 = DIRECTION ( 'NONE',  ( -0.000000000000000000, -0.000000000000000000, 1.000000000000000000 ) ) ;
#16515 = ORIENTED_EDGE ( 'NONE', *, *, #4940, .T. ) ;
#16516 = CARTESIAN_POINT ( 'NONE',  ( -9.015947181032835626E-10, -7.500000000000007994, 8.994950000180315541 ) ) ;
#16517 = ORIENTED_EDGE ( 'NONE', *, *, #4456, .F. ) ;
#16518 = DIRECTION ( 'NONE',  ( -1.000000000000000000, 0.000000000000000000, 0.000000000000000000 ) ) ;
#16519 = CARTESIAN_POINT ( 'NONE',  ( -6.888301780572500199, 16.62983158603121936, -0.3913624998196918447 ) ) ;
#16520 = EDGE_LOOP ( 'NONE', ( #5980, #1132, #16515, #16300 ) ) ;
#16521 = ORIENTED_EDGE ( 'NONE', *, *, #15985, .F. ) ;
#16522 = CARTESIAN_POINT ( 'NONE',  ( 19.99999999999999645, -14.55863677812166124, 63.60407295269099137 ) ) ;
#16523 = CARTESIAN_POINT ( 'NONE',  ( 0.000000000000000000, 39.37110852956814000, 51.51683813304883586 ) ) ;
#16524 = CARTESIAN_POINT ( 'NONE',  ( 30.00000000000000000, -85.00000000000000000, -1.040949779275250179E-14 ) ) ;
#16525 = CARTESIAN_POINT ( 'NONE',  ( 19.99999999999999645, 8.857208570069795783, 71.45313048675087941 ) ) ;
#16526 = EDGE_CURVE ( 'NONE', #2438, #2694, #9599, .T. ) ;
#16527 = DIRECTION ( 'NONE',  ( 1.000000000000000000, 0.000000000000000000, 0.000000000000000000 ) ) ;
#16528 = CARTESIAN_POINT ( 'NONE',  ( 1.491842754445843688, -7.500000000179346316, 18.12541875018031945 ) ) ;
#16529 = CARTESIAN_POINT ( 'NONE',  ( 6.330490856366289165, -9.474249098604506258, 10.84254649971319751 ) ) ;
#16530 = CARTESIAN_POINT ( 'NONE',  ( 0.000000000000000000, 0.000000000000000000, 0.000000000000000000 ) ) ;
#16531 = DIRECTION ( 'NONE',  ( -1.000000000000000000, 0.000000000000000000, 0.000000000000000000 ) ) ;
#16532 = ORIENTED_EDGE ( 'NONE', *, *, #8694, .F. ) ;
#16533 = DIRECTION ( 'NONE',  ( 0.000000000000000000, 1.000000000000000000, -8.673617379884034239E-17 ) ) ;
#16534 = CARTESIAN_POINT ( 'NONE',  ( -2.163827323447878234E-09, -18.00000000000000000, 16.23980000018031333 ) ) ;
#16535 = FACE_OUTER_BOUND ( 'NONE', #3747, .T. ) ;
#16536 = ORIENTED_EDGE ( 'NONE', *, *, #11804, .T. ) ;
#16537 = CARTESIAN_POINT ( 'NONE',  ( 52.50000000000000000, -40.00000000000000000, 0.000000000000000000 ) ) ;
#16538 = ORIENTED_EDGE ( 'NONE', *, *, #13561, .F. ) ;
#16539 = DIRECTION ( 'NONE',  ( -1.000000000000000000, -0.000000000000000000, -0.000000000000000000 ) ) ;
#16540 = CARTESIAN_POINT ( 'NONE',  ( 40.17604362888928904, -15.41257802331652549, 79.36552202533282241 ) ) ;
#16541 = VERTEX_POINT ( 'NONE', #9802 ) ;
#16542 = ORIENTED_EDGE ( 'NONE', *, *, #7419, .T. ) ;
#16543 = CARTESIAN_POINT ( 'NONE',  ( 0.000000000000000000, 0.000000000000000000, 40.00000000000000000 ) ) ;
#16544 = SURFACE_STYLE_USAGE ( .BOTH. , #18344 ) ;
#16545 = DIRECTION ( 'NONE',  ( 0.000000000000000000, 0.000000000000000000, -1.000000000000000000 ) ) ;
#16546 = ADVANCED_FACE ( 'NONE', ( #14688 ), #12563, .T. ) ;
#16547 = DIRECTION ( 'NONE',  ( 0.000000000000000000, 0.000000000000000000, 1.000000000000000000 ) ) ;
#16548 = CARTESIAN_POINT ( 'NONE',  ( -4.248408729364575365, 6.358192988180014105, 15.98395625018031474 ) ) ;
#16549 = CARTESIAN_POINT ( 'NONE',  ( 34.54863082286252052, -117.7057449628014041, -83.06716769817120394 ) ) ;
#16550 = EDGE_CURVE ( 'NONE', #2694, #10147, #19978, .T. ) ;
#16551 = DIRECTION ( 'NONE',  ( 1.000000000000000000, -0.000000000000000000, -0.000000000000000000 ) ) ;
#16552 = CARTESIAN_POINT ( 'NONE',  ( -21.35784117651625280, 26.35784117651607872, -120.0000000000000142 ) ) ;
#16553 = EDGE_CURVE ( 'NONE', #2556, #9451, #1728, .T. ) ;
#16554 = ORIENTED_EDGE ( 'NONE', *, *, #1398, .F. ) ;
#16555 = LINE ( 'NONE', #5414, #401 ) ;
#16556 = ORIENTED_EDGE ( 'NONE', *, *, #13601, .T. ) ;
#16557 = DIRECTION ( 'NONE',  ( -1.000000000000000000, 0.000000000000000000, 0.000000000000000000 ) ) ;
#16558 = DIRECTION ( 'NONE',  ( 1.000000000000000000, 0.000000000000000000, 0.000000000000000000 ) ) ;
#16559 = EDGE_LOOP ( 'NONE', ( #7068, #13843, #2273, #6930 ) ) ;
#16560 = CARTESIAN_POINT ( 'NONE',  ( 50.00000000000000000, -125.0000000000000000, 90.00000000000002842 ) ) ;
#16561 = ORIENTED_EDGE ( 'NONE', *, *, #5463, .T. ) ;
#16562 = DIRECTION ( 'NONE',  ( -1.000000000000000000, 0.000000000000000000, 0.000000000000000000 ) ) ;
#16563 = LINE ( 'NONE', #14284, #602 ) ;
#16564 = EDGE_LOOP ( 'NONE', ( #16931, #9652, #11047, #17897, #14471 ) ) ;
#16565 = CARTESIAN_POINT ( 'NONE',  ( 1.491842756249029289, 7.499999999820664343, -11.11291874981969485 ) ) ;
#16566 = VECTOR ( 'NONE', #20200, 1000.000000000000000 ) ;
#16567 = LINE ( 'NONE', #11394, #18394 ) ;
#16568 = CARTESIAN_POINT ( 'NONE',  ( -9.474249097082500626, 6.330490858644140850, 12.66370350064742922 ) ) ;
#16569 = ORIENTED_EDGE ( 'NONE', *, *, #19576, .T. ) ;
#16570 = CARTESIAN_POINT ( 'NONE',  ( 0.000000000000000000, 0.000000000000000000, 0.000000000000000000 ) ) ;
#16571 = CARTESIAN_POINT ( 'NONE',  ( 0.000000000000000000, 63.85430960833490843, -11.25592921604860663 ) ) ;
#16572 = ORIENTED_EDGE ( 'NONE', *, *, #7027, .T. ) ;
#16573 = CARTESIAN_POINT ( 'NONE',  ( 10.00000000000000178, -113.2094389508847314, -74.86138894033631175 ) ) ;
#16574 = EDGE_CURVE ( 'NONE', #20260, #5709, #13565, .T. ) ;
#16575 = VERTEX_POINT ( 'NONE', #5127 ) ;
#16576 = EDGE_CURVE ( 'NONE', #3596, #16499, #18295, .T. ) ;
#16577 = CARTESIAN_POINT ( 'NONE',  ( -15.25966317163203279, -10.19618095047498052, -1.137543749819686756 ) ) ;
#16578 = FACE_OUTER_BOUND ( 'NONE', #16691, .T. ) ;
#16579 = DIRECTION ( 'NONE',  ( -0.000000000000000000, -0.000000000000000000, 1.000000000000000000 ) ) ;
#16580 = EDGE_LOOP ( 'NONE', ( #4837, #19913, #15212, #5492 ) ) ;
#16581 = DIRECTION ( 'NONE',  ( 0.000000000000000000, 1.000000000000000000, -1.224646799147353207E-16 ) ) ;
#16582 = ADVANCED_FACE ( 'NONE', ( #1455, #7908, #14387, #20829, #8828 ), #7129, .F. ) ;
#16583 = ORIENTED_EDGE ( 'NONE', *, *, #7693, .F. ) ;
#16584 = CARTESIAN_POINT ( 'NONE',  ( 6.250000000000054179, 10.82531754730546147, -43.00000000000000000 ) ) ;
#16585 = EDGE_LOOP ( 'NONE', ( #15990, #6909, #14228, #7354 ) ) ;
#16586 = DIRECTION ( 'NONE',  ( -1.000000000000000000, 0.000000000000000000, 0.000000000000000000 ) ) ;
#16587 = PRODUCT_DEFINITION_SHAPE ( 'NONE', 'NONE',  #20962 ) ;
#16588 = DIRECTION ( 'NONE',  ( -1.000000000000000000, 0.000000000000000000, 0.000000000000000000 ) ) ;
#16589 = APPLICATION_PROTOCOL_DEFINITION ( 'draft international standard', 'automotive_design', 1998, #4399 ) ;
#16590 = CARTESIAN_POINT ( 'NONE',  ( -14.79893867793684059, -2.943691925285399691, 20.15826066884155310 ) ) ;
#16591 = EDGE_CURVE ( 'NONE', #16060, #8227, #587, .T. ) ;
#16592 = VERTEX_POINT ( 'NONE', #7036 ) ;
#16593 = AXIS2_PLACEMENT_3D ( 'NONE', #159, #1561, #17968 ) ;
#16594 = CARTESIAN_POINT ( 'NONE',  ( 19.99999999999999645, 0.000000000000000000, 0.000000000000000000 ) ) ;
#16595 = CARTESIAN_POINT ( 'NONE',  ( 54.64999999999999858, -99.99999999999998579, 5.000000000000000000 ) ) ;
#16596 = ADVANCED_FACE ( 'NONE', ( #3646 ), #18074, .T. ) ;
#16597 = CARTESIAN_POINT ( 'NONE',  ( -14.79893867758296544, 1.779018419858780125E-09, -22.86529191848093490 ) ) ;
#16598 = AXIS2_PLACEMENT_3D ( 'NONE', #8916, #10192, #455 ) ;
#16599 = EDGE_CURVE ( 'NONE', #11681, #9241, #8147, .T. ) ;
#16600 = DIRECTION ( 'NONE',  ( 0.000000000000000000, -0.9790840876823205807, -0.2034560130526446575 ) ) ;
#16601 = CONICAL_SURFACE ( 'NONE', #707, 2.041999999999999815, 1.047197551196591858 ) ;
#16602 = ORIENTED_EDGE ( 'NONE', *, *, #13647, .T. ) ;
#16603 = EDGE_CURVE ( 'NONE', #16876, #6801, #3540, .T. ) ;
#16604 = DIRECTION ( 'NONE',  ( -1.000000000000000000, -0.000000000000000000, -0.000000000000000000 ) ) ;
#16605 = CARTESIAN_POINT ( 'NONE',  ( 2.870125743571138255, 6.929096493489627306, 17.45661250018030941 ) ) ;
#16606 = ORIENTED_EDGE ( 'NONE', *, *, #20737, .T. ) ;
#16607 = CARTESIAN_POINT ( 'NONE',  ( -31.75000000000000000, -10.52399999999999558, 1.288818291422673979E-15 ) ) ;
#16608 = ORIENTED_EDGE ( 'NONE', *, *, #10901, .T. ) ;
#16609 = FACE_OUTER_BOUND ( 'NONE', #9075, .T. ) ;
#16610 = CARTESIAN_POINT ( 'NONE',  ( -18.00000000043040771, -3.580422610670021211, 6.971918750180310376 ) ) ;
#16611 = VERTEX_POINT ( 'NONE', #20060 ) ;
#16612 = VERTEX_POINT ( 'NONE', #8734 ) ;
#16613 = DIRECTION ( 'NONE',  ( 0.000000000000000000, 0.000000000000000000, 1.000000000000000000 ) ) ;
#16614 = VECTOR ( 'NONE', #4627, 1000.000000000000000 ) ;
#16615 = DIRECTION ( 'NONE',  ( -1.000000000000000000, 0.000000000000000000, 0.000000000000000000 ) ) ;
#16616 = FACE_BOUND ( 'NONE', #20101, .T. ) ;
#16617 = AXIS2_PLACEMENT_3D ( 'NONE', #15164, #2128, #11868 ) ;
#16618 =( NAMED_UNIT ( * ) SI_UNIT ( $, .STERADIAN. ) SOLID_ANGLE_UNIT ( ) );
#16619 = CARTESIAN_POINT ( 'NONE',  ( 30.00000000000000000, -40.41646384503856382, 66.42520834682602526 ) ) ;
#16620 = EDGE_CURVE ( 'NONE', #15651, #3116, #4427, .T. ) ;
#16621 = ADVANCED_FACE ( 'NONE', ( #14995 ), #18489, .T. ) ;
#16622 = UNCERTAINTY_MEASURE_WITH_UNIT (LENGTH_MEASURE( 1.000000000000000082E-05 ), #20772, 'distance_accuracy_value', 'NONE');
#16623 = CARTESIAN_POINT ( 'NONE',  ( -6.177131623262581250, 0.000000000000000000, 10.85999999999999410 ) ) ;
#16624 = CARTESIAN_POINT ( 'NONE',  ( -4.248408729364580694, 6.358192988180020322, 3.398856250180315897 ) ) ;
#16625 = VECTOR ( 'NONE', #17826, 1000.000000000000000 ) ;
#16626 = CARTESIAN_POINT ( 'NONE',  ( 7.902369978624323110, 7.902369976724394895, -20.08323475028680605 ) ) ;
#16627 = EDGE_CURVE ( 'NONE', #2326, #1075, #8513, .T. ) ;
#16628 = DIRECTION ( 'NONE',  ( -0.000000000000000000, 0.000000000000000000, 1.000000000000000000 ) ) ;
#16629 = LINE ( 'NONE', #14945, #18487 ) ;
#16630 = CIRCLE ( 'NONE', #1082, 17.50000000000000355 ) ;
#16631 = VECTOR ( 'NONE', #9884, 1000.000000000000000 ) ;
#16632 = EDGE_LOOP ( 'NONE', ( #17087, #9143, #18363, #8353 ) ) ;
#16633 = LINE ( 'NONE', #5083, #6836 ) ;
#16634 = CARTESIAN_POINT ( 'NONE',  ( -6.888301780572501976, 16.62983158603122291, -7.911762499819688266 ) ) ;
#16635 = CARTESIAN_POINT ( 'NONE',  ( 0.000000000000000000, 0.000000000000000000, 0.000000000000000000 ) ) ;
#16636 = CIRCLE ( 'NONE', #6152, 27.60000000002759890 ) ;
#16637 = ORIENTED_EDGE ( 'NONE', *, *, #17627, .T. ) ;
#16638 = DIRECTION ( 'NONE',  ( -1.000000000000000000, 0.000000000000000000, 0.000000000000000000 ) ) ;
#16639 = ORIENTED_EDGE ( 'NONE', *, *, #10266, .F. ) ;
#16640 = CYLINDRICAL_SURFACE ( 'NONE', #16617, 2.649999999999993694 ) ;
#16641 = CARTESIAN_POINT ( 'NONE',  ( 36.99122470214116021, -20.97311120624805625, -70.79638128036988576 ) ) ;
#16642 = EDGE_CURVE ( 'NONE', #8495, #6843, #9171, .T. ) ;
#16643 = VERTEX_POINT ( 'NONE', #14889 ) ;
#16644 = VECTOR ( 'NONE', #14989, 1000.000000000000000 ) ;
#16645 = ORIENTED_EDGE ( 'NONE', *, *, #19092, .F. ) ;
#16646 = CARTESIAN_POINT ( 'NONE',  ( 19.99999999999999645, -31.98952867950285395, -56.39803944231618971 ) ) ;
#16647 = PRESENTATION_STYLE_ASSIGNMENT (( #334 ) ) ;
#16648 = CARTESIAN_POINT ( 'NONE',  ( 19.99999999999999645, -63.17103598352137794, 16.33561182745118501 ) ) ;
#16649 = VECTOR ( 'NONE', #17368, 1000.000000000000000 ) ;
#16650 = AXIS2_PLACEMENT_3D ( 'NONE', #114, #11145, #9665 ) ;
#16651 = DIRECTION ( 'NONE',  ( -1.000000000000000000, -0.000000000000000000, -0.000000000000000000 ) ) ;
#16652 = AXIS2_PLACEMENT_3D ( 'NONE', #18237, #6990, #19919 ) ;
#16653 = CARTESIAN_POINT ( 'NONE',  ( -6.929096493489625530, 2.870125743571138255, -13.17463749981968846 ) ) ;
#16654 = FACE_OUTER_BOUND ( 'NONE', #16032, .T. ) ;
#16655 = LINE ( 'NONE', #8800, #10177 ) ;
#16656 = CARTESIAN_POINT ( 'NONE',  ( 19.99999999999999645, -48.70996102988652154, -42.79495875147824790 ) ) ;
#16657 = ORIENTED_EDGE ( 'NONE', *, *, #10683, .F. ) ;
#16658 = CARTESIAN_POINT ( 'NONE',  ( -24.99999999999999289, 230.0000000000000000, 84.99999999999998579 ) ) ;
#16659 = VERTEX_POINT ( 'NONE', #483 ) ;
#16660 = CARTESIAN_POINT ( 'NONE',  ( 16.62983158603122291, 6.888301780572502864, 1.964887500180312330 ) ) ;
#16661 = CARTESIAN_POINT ( 'NONE',  ( -16.87108763463411165, -13.40169213801851278, 74.74090047603390019 ) ) ;
#16662 = AXIS2_PLACEMENT_3D ( 'NONE', #14461, #10161, #7072 ) ;
#16663 = ORIENTED_EDGE ( 'NONE', *, *, #18800, .F. ) ;
#16664 = ADVANCED_FACE ( 'NONE', ( #13305 ), #2375, .F. ) ;
#16665 = DIRECTION ( 'NONE',  ( 0.000000000000000000, 0.000000000000000000, 1.000000000000000000 ) ) ;
#16666 = ORIENTED_EDGE ( 'NONE', *, *, #18562, .F. ) ;
#16667 = CARTESIAN_POINT ( 'NONE',  ( 8.900000000000046541, 10.82531754730546147, 169.0000000000000000 ) ) ;
#16668 = DIRECTION ( 'NONE',  ( -1.000000000000000000, 0.000000000000000000, 0.000000000000000000 ) ) ;
#16669 = EDGE_CURVE ( 'NONE', #2302, #19812, #364, .T. ) ;
#16670 = AXIS2_PLACEMENT_3D ( 'NONE', #1592, #6543, #3363 ) ;
#16671 = VECTOR ( 'NONE', #18286, 1000.000000000000000 ) ;
#16672 = ORIENTED_EDGE ( 'NONE', *, *, #18299, .F. ) ;
#16673 = CIRCLE ( 'NONE', #11933, 65.24900000006526568 ) ;
#16674 = CARTESIAN_POINT ( 'NONE',  ( -4.248408729364577141, 6.358192988180014993, -12.29104374981969094 ) ) ;
#16675 = CARTESIAN_POINT ( 'NONE',  ( 12.72792206288790773, 12.72792205982779912, -8.049174999819690868 ) ) ;
#16676 = DIRECTION ( 'NONE',  ( -1.000000000000000000, 0.000000000000000000, 0.000000000000000000 ) ) ;
#16677 = CARTESIAN_POINT ( 'NONE',  ( 19.99999999999999645, -43.56693332842820610, 48.57318520917490190 ) ) ;
#16678 = CARTESIAN_POINT ( 'NONE',  ( 6.330490856366294494, -9.474249098604513364, 17.96526600064742851 ) ) ;
#16679 = AXIS2_PLACEMENT_3D ( 'NONE', #7257, #2297, #4305 ) ;
#16680 = EDGE_LOOP ( 'NONE', ( #16882, #17592 ) ) ;
#16681 = DIRECTION ( 'NONE',  ( 1.000000000000000000, 0.000000000000000000, 0.000000000000000000 ) ) ;
#16682 = CARTESIAN_POINT ( 'NONE',  ( 10.00000000000000178, -40.41646384503850697, -66.42520834682601105 ) ) ;
#16683 = VERTEX_POINT ( 'NONE', #6816 ) ;
#16684 = CARTESIAN_POINT ( 'NONE',  ( 21.45900938229203447, -1.326995226329880762, -84.99999999999998579 ) ) ;
#16685 = ORIENTED_EDGE ( 'NONE', *, *, #12003, .T. ) ;
#16686 = CARTESIAN_POINT ( 'NONE',  ( -18.00000000000000000, 2.163826221265758884E-09, 9.171050000180313688 ) ) ;
#16687 = CARTESIAN_POINT ( 'NONE',  ( -52.49999999999999289, -130.0000000000000000, 0.000000000000000000 ) ) ;
#16688 = DIRECTION ( 'NONE',  ( 1.000000000000000000, 0.000000000000000000, 0.000000000000000000 ) ) ;
#16689 = AXIS2_PLACEMENT_3D ( 'NONE', #6183, #4493, #7567 ) ;
#16690 = AXIS2_PLACEMENT_3D ( 'NONE', #17192, #19094, #13899 ) ;
#16691 = EDGE_LOOP ( 'NONE', ( #10856, #17981, #19707, #14551 ) ) ;
#16692 = ORIENTED_EDGE ( 'NONE', *, *, #2964, .T. ) ;
#16693 = AXIS2_PLACEMENT_3D ( 'NONE', #4052, #16993, #10533 ) ;
#16694 = CARTESIAN_POINT ( 'NONE',  ( 19.99999999999999645, 31.98952867950324830, 56.39803944231596944 ) ) ;
#16695 = AXIS2_PLACEMENT_3D ( 'NONE', #15395, #10521, #13288 ) ;
#16696 = EDGE_LOOP ( 'NONE', ( #6357, #2917, #6827, #7858, #7560 ) ) ;
#16697 = CARTESIAN_POINT ( 'NONE',  ( 0.000000000000000000, 10.77748419466781726, -63.93680186330462334 ) ) ;
#16698 = ADVANCED_FACE ( 'NONE', ( #13611 ), #3955, .F. ) ;
#16699 = CARTESIAN_POINT ( 'NONE',  ( 10.00000000000000178, -113.2094389508847172, 74.86138894033631175 ) ) ;
#16700 = CIRCLE ( 'NONE', #2493, 72.00000000007199219 ) ;
#16701 = CARTESIAN_POINT ( 'NONE',  ( 1.779017513685136568E-09, 14.79893867758297610, 13.38404191884154670 ) ) ;
#16702 = AXIS2_PLACEMENT_3D ( 'NONE', #14302, #14201, #2740 ) ;
#16703 = VECTOR ( 'NONE', #20498, 1000.000000000000000 ) ;
#16704 = ORIENTED_EDGE ( 'NONE', *, *, #7534, .T. ) ;
#16705 = DIRECTION ( 'NONE',  ( 1.000000000000000000, 0.000000000000000000, 0.000000000000000000 ) ) ;
#16706 = ORIENTED_EDGE ( 'NONE', *, *, #19954, .F. ) ;
#16707 = VECTOR ( 'NONE', #3103, 1000.000000000000000 ) ;
#16708 = EDGE_CURVE ( 'NONE', #8862, #12428, #6116, .T. ) ;
#16709 = CARTESIAN_POINT ( 'NONE',  ( -31.74999999999995737, 0.000000000000000000, 0.000000000000000000 ) ) ;
#16710 = AXIS2_PLACEMENT_3D ( 'NONE', #20897, #4784, #11978 ) ;
#16711 = CARTESIAN_POINT ( 'NONE',  ( -13.67243654642775041, 5.663308650141531508, -22.27622941848092708 ) ) ;
#16712 = VECTOR ( 'NONE', #12979, 1000.000000000000000 ) ;
#16713 = CARTESIAN_POINT ( 'NONE',  ( 9.999999999999998224, 51.96384592647199696, 49.83732252579632416 ) ) ;
#16714 = ORIENTED_EDGE ( 'NONE', *, *, #8322, .F. ) ;
#16715 = CARTESIAN_POINT ( 'NONE',  ( 0.000000000000000000, -70.29359119158496583, 15.58239511117263554 ) ) ;
#16716 = CARTESIAN_POINT ( 'NONE',  ( 2.500000000000000000, -1.178949249685218748, -2.041999999999998039 ) ) ;
#16717 = AXIS2_PLACEMENT_3D ( 'NONE', #9053, #15092, #16892 ) ;
#16718 = ORIENTED_EDGE ( 'NONE', *, *, #3369, .T. ) ;
#16719 = CARTESIAN_POINT ( 'NONE',  ( 1.491842754445843688, -7.500000000179346316, 8.700418750180315186 ) ) ;
#16720 = ORIENTED_EDGE ( 'NONE', *, *, #11064, .F. ) ;
#16721 = FACE_OUTER_BOUND ( 'NONE', #1562, .T. ) ;
#16722 = CARTESIAN_POINT ( 'NONE',  ( -17.99999999999999645, 2.163826221265758470E-09, 7.266450000180311619 ) ) ;
#16723 = ORIENTED_EDGE ( 'NONE', *, *, #11240, .T. ) ;
#16724 = ORIENTED_EDGE ( 'NONE', *, *, #13765, .T. ) ;
#16725 = AXIS2_PLACEMENT_3D ( 'NONE', #19735, #19427, #11682 ) ;
#16726 = FACE_OUTER_BOUND ( 'NONE', #3152, .T. ) ;
#16727 = ADVANCED_FACE ( 'NONE', ( #18381 ), #3848, .F. ) ;
#16728 = AXIS2_PLACEMENT_3D ( 'NONE', #7433, #20475, #11148 ) ;
#16729 = ADVANCED_FACE ( 'NONE', ( #10437 ), #1048, .T. ) ;
#16730 = CARTESIAN_POINT ( 'NONE',  ( 19.99999999999999645, 70.29359119158506530, -15.58239511117215059 ) ) ;
#16731 = DIRECTION ( 'NONE',  ( -1.000000000000000000, 0.000000000000000000, 0.000000000000000000 ) ) ;
#16732 =( LENGTH_UNIT ( ) NAMED_UNIT ( * ) SI_UNIT ( .MILLI., .METRE. ) );
#16733 = CARTESIAN_POINT ( 'NONE',  ( -1.491842754445842800, 7.500000000179346316, -14.86208124981968481 ) ) ;
#16735 = ADVANCED_FACE ( 'NONE', ( #12229 ), #5753, .T. ) ;
#16734 = DIRECTION ( 'NONE',  ( 0.000000000000000000, 0.000000000000000000, 1.000000000000000000 ) ) ;
#16736 = CARTESIAN_POINT ( 'NONE',  ( -1.491842756249033064, -7.499999999820668783, -9.560518749819690854 ) ) ;
#16737 = CARTESIAN_POINT ( 'NONE',  ( -2.222972768810836275, 11.17563879758427525, -21.55589100028680249 ) ) ;
#16738 = DIRECTION ( 'NONE',  ( 0.000000000000000000, 0.000000000000000000, 1.000000000000000000 ) ) ;
#16739 = CARTESIAN_POINT ( 'NONE',  ( 30.00000000000000000, -122.0000000000000000, -6.368163355566234804E-15 ) ) ;
#16740 = AXIS2_PLACEMENT_3D ( 'NONE', #2011, #11964, #16734 ) ;
#16741 = ORIENTED_EDGE ( 'NONE', *, *, #9769, .F. ) ;
#16742 = CARTESIAN_POINT ( 'NONE',  ( -9.850000000000012079, 3.245314017740478073E-16, 126.0000000000000000 ) ) ;
#16743 = CARTESIAN_POINT ( 'NONE',  ( 18.00000000000000000, -2.163824016901520184E-09, -4.966449999819686489 ) ) ;
#16744 = CARTESIAN_POINT ( 'NONE',  ( 9.999999999999998224, 27.80658314415226684, 66.41380830714133765 ) ) ;
#16745 = EDGE_CURVE ( 'NONE', #13598, #1332, #7463, .T. ) ;
#16746 = EDGE_LOOP ( 'NONE', ( #1525, #13699, #16834, #7538 ) ) ;
#16747 = EDGE_CURVE ( 'NONE', #19634, #9479, #15615, .T. ) ;
#16748 = FACE_OUTER_BOUND ( 'NONE', #13997, .T. ) ;
#16749 = ORIENTED_EDGE ( 'NONE', *, *, #19203, .T. ) ;
#16750 = DIRECTION ( 'NONE',  ( 0.000000000000000000, 0.000000000000000000, 1.000000000000000000 ) ) ;
#16751 = CARTESIAN_POINT ( 'NONE',  ( 5.200000000000002842, 3.061616997868383634E-16, -2.500000000000000444 ) ) ;
#16752 = ORIENTED_EDGE ( 'NONE', *, *, #14250, .F. ) ;
#16753 = VERTEX_POINT ( 'NONE', #1005 ) ;
#16754 = PRODUCT_DEFINITION_FORMATION_WITH_SPECIFIED_SOURCE ( 'ANY', '', #12039, .NOT_KNOWN. ) ;
#16755 = FACE_OUTER_BOUND ( 'NONE', #7222, .T. ) ;
#16756 = ADVANCED_FACE ( 'NONE', ( #1115 ), #18700, .F. ) ;
#16757 = CARTESIAN_POINT ( 'NONE',  ( 19.99999999999999645, 19.38316218894212639, 61.87375713200996330 ) ) ;
#16758 = STYLED_ITEM ( 'NONE', ( #7350 ), #10589 ) ;
#16759 = LINE ( 'NONE', #5722, #16381 ) ;
#16760 = CARTESIAN_POINT ( 'NONE',  ( 6.358192987158590270, -4.248408730893245000, -8.167606249819691300 ) ) ;
#16761 = DIRECTION ( 'NONE',  ( -1.000000000000000000, 0.000000000000000000, -0.000000000000000000 ) ) ;
#16762 = FILL_AREA_STYLE_COLOUR ( '', #11507 ) ;
#16763 = CARTESIAN_POINT ( 'NONE',  ( 29.74873734152916782, 24.74873734152916072, -120.0000000000000142 ) ) ;
#16764 = DIRECTION ( 'NONE',  ( 0.000000000000000000, 0.000000000000000000, 1.000000000000000000 ) ) ;
#16765 = ORIENTED_EDGE ( 'NONE', *, *, #3635, .T. ) ;
#16766 = CARTESIAN_POINT ( 'NONE',  ( 6.929096494179683319, 2.870125741905213079, 6.049637500180313765 ) ) ;
#16767 = AXIS2_PLACEMENT_3D ( 'NONE', #1105, #886, #12010 ) ;
#16768 = ORIENTED_EDGE ( 'NONE', *, *, #10045, .T. ) ;
#16769 = CARTESIAN_POINT ( 'NONE',  ( 18.00000000043041126, 3.580422610670019434, 11.68441875018031517 ) ) ;
#16770 = DIRECTION ( 'NONE',  ( -1.000000000000000000, -0.000000000000000000, -0.000000000000000000 ) ) ;
#16771 = ORIENTED_EDGE ( 'NONE', *, *, #18699, .T. ) ;
#16772 = CARTESIAN_POINT ( 'NONE',  ( -30.00000000000000000, 36.35083268962915781, 50.00000000000000000 ) ) ;
#16773 = VERTEX_POINT ( 'NONE', #2593 ) ;
#16774 = VECTOR ( 'NONE', #533, 1000.000000000000000 ) ;
#16775 = PRODUCT_DEFINITION_SHAPE ( 'NONE', 'NONE',  #20966 ) ;
#16776 = CARTESIAN_POINT ( 'NONE',  ( 3.599999999999913936, -10.82531754730554496, 46.00000000000000711 ) ) ;
#16777 = DIRECTION ( 'NONE',  ( 0.000000000000000000, 0.000000000000000000, 1.000000000000000000 ) ) ;
#16778 = ORIENTED_EDGE ( 'NONE', *, *, #11038, .F. ) ;
#16779 = LINE ( 'NONE', #2267, #605 ) ;
#16780 = CARTESIAN_POINT ( 'NONE',  ( -15.25966317163202923, -10.19618095047497874, -3.042143749819689713 ) ) ;
#16781 = CARTESIAN_POINT ( 'NONE',  ( 3.999999999999990674, -2.309401076758548221, -0.3572655899081733644 ) ) ;
#16782 = CIRCLE ( 'NONE', #6302, 65.24900000006525147 ) ;
#16783 = CARTESIAN_POINT ( 'NONE',  ( 19.99999999999999645, 27.80658314415225973, 66.41380830714133765 ) ) ;
#16784 = CARTESIAN_POINT ( 'NONE',  ( -4.276731812588566939, 10.32494394809439875, 13.54729725064743384 ) ) ;
#16785 = ORIENTED_EDGE ( 'NONE', *, *, #10912, .T. ) ;
#16786 = AXIS2_PLACEMENT_3D ( 'NONE', #15418, #10442, #8833 ) ;
#16787 = AXIS2_PLACEMENT_3D ( 'NONE', #19811, #12374, #8679 ) ;
#16788 = DIRECTION ( 'NONE',  ( 1.000000000000000000, -0.000000000000000000, -0.000000000000000000 ) ) ;
#16789 = EDGE_CURVE ( 'NONE', #20492, #1625, #12550, .T. ) ;
#16790 = CARTESIAN_POINT ( 'NONE',  ( 19.99999999999999645, -24.01204443665229604, 60.22865198596116443 ) ) ;
#16791 = ORIENTED_EDGE ( 'NONE', *, *, #18268, .T. ) ;
#16792 = LINE ( 'NONE', #18703, #14882 ) ;
#16793 = ORIENTED_EDGE ( 'NONE', *, *, #1991, .F. ) ;
#16794 = CARTESIAN_POINT ( 'NONE',  ( -18.00000000043041126, -3.580422610670022099, -0.5484812498196891539 ) ) ;
#16795 = CIRCLE ( 'NONE', #2634, 72.00000000007199219 ) ;
#16796 = CARTESIAN_POINT ( 'NONE',  ( -12.50000000000000533, 0.000000000000000000, 46.00000000000000711 ) ) ;
#16797 = DIRECTION ( 'NONE',  ( 0.000000000000000000, 0.000000000000000000, 1.000000000000000000 ) ) ;
#16798 = EDGE_LOOP ( 'NONE', ( #18091, #14752, #10769, #2043 ) ) ;
#16799 = CARTESIAN_POINT ( 'NONE',  ( 0.000000000000000000, -24.01204443665229604, 60.22865198596116443 ) ) ;
#16800 = ORIENTED_EDGE ( 'NONE', *, *, #15463, .F. ) ;
#16801 = PLANE ( 'NONE',  #16301 ) ;
#16802 = VECTOR ( 'NONE', #19904, 1000.000000000000000 ) ;
#16803 = VERTEX_POINT ( 'NONE', #9060 ) ;
#16804 = DIRECTION ( 'NONE',  ( 1.000000000000000000, 0.000000000000000000, 0.000000000000000000 ) ) ;
#16805 = AXIS2_PLACEMENT_3D ( 'NONE', #1888, #16105, #16403 ) ;
#16806 = CIRCLE ( 'NONE', #4960, 2.055000000000000160 ) ;
#16807 = STYLED_ITEM ( 'NONE', ( #7635 ), #11209 ) ;
#16808 = VERTEX_POINT ( 'NONE', #2485 ) ;
#16809 = FACE_OUTER_BOUND ( 'NONE', #2060, .T. ) ;
#16810 = CIRCLE ( 'NONE', #11058, 65.24900000006525147 ) ;
#16811 = CARTESIAN_POINT ( 'NONE',  ( 0.000000000000000000, 0.000000000000000000, 0.000000000000000000 ) ) ;
#16812 = CONTEXT_DEPENDENT_SHAPE_REPRESENTATION ( #15631, #2046 ) ;
#16813 = CARTESIAN_POINT ( 'NONE',  ( -10.46442989454075878, -10.46442989202484242, 9.849666918841547769 ) ) ;
#16814 = ORIENTED_EDGE ( 'NONE', *, *, #9631, .T. ) ;
#16815 = CIRCLE ( 'NONE', #11402, 27.60000000002759535 ) ;
#16816 = EDGE_CURVE ( 'NONE', #12290, #857, #12546, .T. ) ;
#16817 = AXIS2_PLACEMENT_3D ( 'NONE', #19262, #4742, #9920 ) ;
#16818 = CARTESIAN_POINT ( 'NONE',  ( 0.000000000000000000, 0.000000000000000000, 46.00000000000000711 ) ) ;
#16819 = ORIENTED_EDGE ( 'NONE', *, *, #15149, .T. ) ;
#16820 = CARTESIAN_POINT ( 'NONE',  ( 6.249999999999902300, -10.82531754730554496, 43.00000000000000000 ) ) ;
#16821 = CIRCLE ( 'NONE', #3288, 7.500000000000000000 ) ;
#16822 = CARTESIAN_POINT ( 'NONE',  ( 14.79893867758296544, -1.779016607511491977E-09, -27.57779191848093703 ) ) ;
#16823 = CARTESIAN_POINT ( 'NONE',  ( -2.271448787322325728E-15, -4.618802153517061804, -5.599999999999999645 ) ) ;
#16824 = EDGE_CURVE ( 'NONE', #3130, #6711, #15926, .T. ) ;
#16825 = EDGE_LOOP ( 'NONE', ( #20432, #11356 ) ) ;
#16826 = CARTESIAN_POINT ( 'NONE',  ( 19.99999999999999645, -31.17893654894269773, 57.31758819669160232 ) ) ;
#16827 = CARTESIAN_POINT ( 'NONE',  ( 6.250000000000054179, 10.82531754730546147, 46.00000000000000711 ) ) ;
#16828 = VECTOR ( 'NONE', #2093, 1000.000000000000114 ) ;
#16829 = EDGE_LOOP ( 'NONE', ( #15328, #13704, #662, #19966 ) ) ;
#16830 = DIRECTION ( 'NONE',  ( 0.000000000000000000, -1.000000000000000000, -0.000000000000000000 ) ) ;
#16831 = ORIENTED_EDGE ( 'NONE', *, *, #8280, .F. ) ;
#16832 = DIRECTION ( 'NONE',  ( -1.000000000000000000, 0.000000000000000000, 0.000000000000000000 ) ) ;
#16833 = CARTESIAN_POINT ( 'NONE',  ( -2.163827323447877821E-09, -17.99999999999999645, 14.33520000018031126 ) ) ;
#16834 = ORIENTED_EDGE ( 'NONE', *, *, #9875, .T. ) ;
#16835 = ORIENTED_EDGE ( 'NONE', *, *, #20027, .T. ) ;
#16836 = DIRECTION ( 'NONE',  ( 0.000000000000000000, -0.3984010898462486683, 0.9172113015054499385 ) ) ;
#16837 = AXIS2_PLACEMENT_3D ( 'NONE', #13207, #11611, #18086 ) ;
#16838 = AXIS2_PLACEMENT_3D ( 'NONE', #9068, #13938, #20395 ) ;
#16839 = DIRECTION ( 'NONE',  ( 1.000000000000000000, 1.836909530733573776E-16, 0.000000000000000000 ) ) ;
#16840 = DIRECTION ( 'NONE',  ( -0.000000000000000000, -0.000000000000000000, 1.000000000000000000 ) ) ;
#16841 = SHAPE_REPRESENTATION_RELATIONSHIP ( 'NONE' , 'NONE' ,  #12383, #15250 ) ;
#16842 = CARTESIAN_POINT ( 'NONE',  ( 0.000000000000000000, -35.35772184876843482, -54.34979580218228534 ) ) ;
#16843 = PRODUCT_DEFINITION_CONTEXT ( 'detailed design', #316, 'design' ) ;
#16844 = CARTESIAN_POINT ( 'NONE',  ( -6.929096493489632635, 2.870125743571140919, 2.515262500180314387 ) ) ;
#16845 = VECTOR ( 'NONE', #19157, 1000.000000000000000 ) ;
#16846 = CARTESIAN_POINT ( 'NONE',  ( -9.474249097082497073, 6.330490858644137298, -22.73401600028680747 ) ) ;
#16847 = EDGE_CURVE ( 'NONE', #13848, #17803, #12197, .T. ) ;
#16848 = AXIS2_PLACEMENT_3D ( 'NONE', #7367, #6090, #17235 ) ;
#16849 = CYLINDRICAL_SURFACE ( 'NONE', #2626, 11.49999999999999467 ) ;
#16850 = EDGE_CURVE ( 'NONE', #19897, #13895, #7564, .T. ) ;
#16851 = CIRCLE ( 'NONE', #19888, 72.00000000007199219 ) ;
#16852 = ORIENTED_EDGE ( 'NONE', *, *, #4192, .F. ) ;
#16853 = FACE_OUTER_BOUND ( 'NONE', #3849, .T. ) ;
#16854 = EDGE_CURVE ( 'NONE', #1518, #10611, #13551, .T. ) ;
#16855 = CARTESIAN_POINT ( 'NONE',  ( -3.580422610670018546, 18.00000000043041126, 1.807768750180311468 ) ) ;
#16856 = CARTESIAN_POINT ( 'NONE',  ( 19.99999999999999645, 38.22257254261820947, -61.01667762370099979 ) ) ;
#16857 = ORIENTED_EDGE ( 'NONE', *, *, #4539, .T. ) ;
#16858 = CARTESIAN_POINT ( 'NONE',  ( -52.00000000000000000, -99.99999999999998579, 5.000000000000000000 ) ) ;
#16859 = VERTEX_POINT ( 'NONE', #2693 ) ;
#16860 = FACE_OUTER_BOUND ( 'NONE', #6965, .T. ) ;
#16861 = CARTESIAN_POINT ( 'NONE',  ( -31.74999999999995737, 0.000000000000000000, 2.500000000000000444 ) ) ;
#16862 = ORIENTED_EDGE ( 'NONE', *, *, #7519, .T. ) ;
#16863 = ADVANCED_FACE ( 'NONE', ( #20384 ), #12345, .T. ) ;
#16864 = ORIENTED_EDGE ( 'NONE', *, *, #4009, .T. ) ;
#16865 = CARTESIAN_POINT ( 'NONE',  ( -30.00000000000000000, 40.00000000000000000, -120.0000000000000142 ) ) ;
#16866 = PRODUCT_RELATED_PRODUCT_CATEGORY ( 'part', '', ( #3902 ) ) ;
#16867 = LINE ( 'NONE', #19828, #20414 ) ;
#16868 = CARTESIAN_POINT ( 'NONE',  ( -12.50000000000000533, 0.000000000000000000, -43.00000000000000000 ) ) ;
#16869 = EDGE_CURVE ( 'NONE', #9681, #5222, #4384, .T. ) ;
#16870 = CARTESIAN_POINT ( 'NONE',  ( 2.870125741905211747, -6.929096494179675325, -7.284012499819688458 ) ) ;
#16871 = LINE ( 'NONE', #3619, #8467 ) ;
#16872 = FACE_OUTER_BOUND ( 'NONE', #1602, .T. ) ;
#16873 = CARTESIAN_POINT ( 'NONE',  ( 6.250000000000054179, 10.82531754730546147, -40.00000000000000000 ) ) ;
#16874 = DIRECTION ( 'NONE',  ( -1.000000000000000000, -0.000000000000000000, -0.000000000000000000 ) ) ;
#16875 = EDGE_CURVE ( 'NONE', #1099, #11750, #4412, .T. ) ;
#16876 = VERTEX_POINT ( 'NONE', #7351 ) ;
#16877 = CARTESIAN_POINT ( 'NONE',  ( 9.015937996181842420E-10, 7.500000000000007994, 4.282450000180314298 ) ) ;
#16878 = ADVANCED_FACE ( 'NONE', ( #12129 ), #17320, .T. ) ;
#16879 = EDGE_LOOP ( 'NONE', ( #4012, #15236, #18034, #9651 ) ) ;
#16880 = CARTESIAN_POINT ( 'NONE',  ( 3.580422610670020322, -18.00000000043041126, 4.615668750180313751 ) ) ;
#16881 = DIRECTION ( 'NONE',  ( -1.000000000000000000, 0.000000000000000000, 0.000000000000000000 ) ) ;
#16882 = ORIENTED_EDGE ( 'NONE', *, *, #6200, .T. ) ;
#16883 = CARTESIAN_POINT ( 'NONE',  ( -2.500000000000002220, 3.061616997868386099E-16, -25.03750572909317285 ) ) ;
#16884 = VERTEX_POINT ( 'NONE', #15729 ) ;
#16885 = EDGE_CURVE ( 'NONE', #2292, #1859, #7101, .T. ) ;
#16886 = CARTESIAN_POINT ( 'NONE',  ( -31.74999999999995737, 0.000000000000000000, 4.250000000000000000 ) ) ;
#16887 = CARTESIAN_POINT ( 'NONE',  ( 0.000000000000000000, -65.23577793412343340, -1.313498510942392450 ) ) ;
#16888 = VERTEX_POINT ( 'NONE', #17435 ) ;
#16889 = FACE_OUTER_BOUND ( 'NONE', #20720, .T. ) ;
#16890 = DIRECTION ( 'NONE',  ( -0.000000000000000000, 0.000000000000000000, 1.000000000000000000 ) ) ;
#16891 = CARTESIAN_POINT ( 'NONE',  ( -3.580422614997674557, -17.99999999956957808, -13.64526874981969584 ) ) ;
#16892 = DIRECTION ( 'NONE',  ( -1.000000000000000000, 0.000000000000000000, 0.000000000000000000 ) ) ;
#16893 = CARTESIAN_POINT ( 'NONE',  ( -7.500000000000002665, -1.491842754878804023, 14.21676875008778751 ) ) ;
#16894 = CARTESIAN_POINT ( 'NONE',  ( -7.902369978624331104, -7.902369976724401113, -17.67301524935258072 ) ) ;
#16895 = CIRCLE ( 'NONE', #1347, 2.500000000000000444 ) ;
#16896 = ORIENTED_EDGE ( 'NONE', *, *, #14919, .T. ) ;
#16897 = ADVANCED_FACE ( 'NONE', ( #4056 ), #13831, .T. ) ;
#16898 = DIRECTION ( 'NONE',  ( 1.000000000000000000, 0.000000000000000000, 0.000000000000000000 ) ) ;
#16899 = DIRECTION ( 'NONE',  ( 0.000000000000000000, 0.000000000000000000, -1.000000000000000000 ) ) ;
#16900 = ORIENTED_EDGE ( 'NONE', *, *, #7732, .T. ) ;
#16901 = CARTESIAN_POINT ( 'NONE',  ( 21.25854252069020589, -3.402546668908722705, -82.74447975664146782 ) ) ;
#16902 = ORIENTED_EDGE ( 'NONE', *, *, #15614, .F. ) ;
#16903 = CARTESIAN_POINT ( 'NONE',  ( -17.99999999956958519, 3.580422614997674113, 9.465581250180312267 ) ) ;
#16904 = DIRECTION ( 'NONE',  ( 1.000000000000000000, 0.000000000000000000, 0.000000000000000000 ) ) ;
#16905 = CARTESIAN_POINT ( 'NONE',  ( 2.500000000000000000, 2.357898499370431722, -2.818925648462311528E-15 ) ) ;
#16906 = ORIENTED_EDGE ( 'NONE', *, *, #3954, .T. ) ;
#16907 = CARTESIAN_POINT ( 'NONE',  ( 0.000000000000000000, 0.000000000000000000, 4.000000000000000000 ) ) ;
#16908 = ORIENTED_EDGE ( 'NONE', *, *, #11919, .F. ) ;
#16909 = CARTESIAN_POINT ( 'NONE',  ( -4.248408729364580694, 6.358192988180020322, 12.82385625018031483 ) ) ;
#16910 = VERTEX_POINT ( 'NONE', #19317 ) ;
#16911 = ADVANCED_FACE ( 'NONE', ( #3411 ), #14659, .T. ) ;
#16912 = ORIENTED_EDGE ( 'NONE', *, *, #7299, .T. ) ;
#16913 = CARTESIAN_POINT ( 'NONE',  ( 50.00000000000000000, 31.35083268962917558, 84.99999999999998579 ) ) ;
#16914 = DIRECTION ( 'NONE',  ( -1.000000000000000000, -0.000000000000000000, -0.000000000000000000 ) ) ;
#16915 = CARTESIAN_POINT ( 'NONE',  ( 2.943691928843431782, 14.79893867722910628, 23.10357316884154599 ) ) ;
#16916 = ORIENTED_EDGE ( 'NONE', *, *, #18566, .T. ) ;
#16917 = CARTESIAN_POINT ( 'NONE',  ( 2.500000000000000000, 1.768423874527822681, -1.021000000000002794 ) ) ;
#16918 = DIRECTION ( 'NONE',  ( 1.000000000000000000, 0.000000000000000000, 0.000000000000000000 ) ) ;
#16919 = CARTESIAN_POINT ( 'NONE',  ( -16.62983158603121936, -6.888301780572499311, 16.10238750018030984 ) ) ;
#16920 = DIRECTION ( 'NONE',  ( 0.000000000000000000, 0.000000000000000000, -1.000000000000000000 ) ) ;
#16921 = ORIENTED_EDGE ( 'NONE', *, *, #3170, .F. ) ;
#16922 = CARTESIAN_POINT ( 'NONE',  ( 6.250000000000054179, 10.82531754730546147, 46.00000000000000711 ) ) ;
#16923 = DIRECTION ( 'NONE',  ( 0.000000000000000000, 0.000000000000000000, 1.000000000000000000 ) ) ;
#16924 = VERTEX_POINT ( 'NONE', #1538 ) ;
#16925 = CYLINDRICAL_SURFACE ( 'NONE', #14315, 72.00000000007199219 ) ;
#16926 = ORIENTED_EDGE ( 'NONE', *, *, #18612, .F. ) ;
#16927 = CYLINDRICAL_SURFACE ( 'NONE', #1762, 72.00000000007199219 ) ;
#16928 = CARTESIAN_POINT ( 'NONE',  ( 3.580422610670019878, -18.00000000043040771, 14.04066875018031091 ) ) ;
#16929 = EDGE_CURVE ( 'NONE', #17230, #10641, #14565, .T. ) ;
#16930 = ORIENTED_EDGE ( 'NONE', *, *, #1322, .F. ) ;
#16931 = ORIENTED_EDGE ( 'NONE', *, *, #5284, .F. ) ;
#16932 = FACE_OUTER_BOUND ( 'NONE', #12649, .T. ) ;
#16933 = AXIS2_PLACEMENT_3D ( 'NONE', #8945, #7676, #10959 ) ;
#16934 = DIRECTION ( 'NONE',  ( -1.000000000000000000, 0.000000000000000000, 0.000000000000000000 ) ) ;
#16935 = LINE ( 'NONE', #8877, #18014 ) ;
#16936 = SHAPE_REPRESENTATION_RELATIONSHIP ( 'NONE' , 'NONE' ,  #2344, #14262 ) ;
#16937 = CARTESIAN_POINT ( 'NONE',  ( 7.500000000000009770, 1.491842754878799138, -12.50583124991220707 ) ) ;
#16938 =( NAMED_UNIT ( * ) SI_UNIT ( $, .STERADIAN. ) SOLID_ANGLE_UNIT ( ) );
#16939 = CARTESIAN_POINT ( 'NONE',  ( -1.491842754445842800, 7.500000000179346316, -5.437081249819685880 ) ) ;
#16940 = CIRCLE ( 'NONE', #2054, 200.0000000000000000 ) ;
#16941 = CYLINDRICAL_SURFACE ( 'NONE', #20561, 27.60000000002760245 ) ;
#16942 = CARTESIAN_POINT ( 'NONE',  ( 6.330490856366289165, -9.474249098604506258, -8.007453500286802139 ) ) ;
#16943 = PRODUCT_DEFINITION_SHAPE ( 'NONE', 'NONE',  #20949 ) ;
#16944 = CARTESIAN_POINT ( 'NONE',  ( 19.99999999999999645, 0.000000000000000000, 0.000000000000000000 ) ) ;
#16945 = VERTEX_POINT ( 'NONE', #14470 ) ;
#16946 = DIRECTION ( 'NONE',  ( -0.000000000000000000, -0.000000000000000000, -1.000000000000000000 ) ) ;
#16947 = CARTESIAN_POINT ( 'NONE',  ( 16.62983158437509346, -6.888301784570739272, -4.377387499819689332 ) ) ;
#16948 = FACE_BOUND ( 'NONE', #14411, .T. ) ;
#16949 = VERTEX_POINT ( 'NONE', #17747 ) ;
#16950 = DIRECTION ( 'NONE',  ( 0.000000000000000000, 0.000000000000000000, -1.000000000000000000 ) ) ;
#16951 = VERTEX_POINT ( 'NONE', #12872 ) ;
#16952 = CARTESIAN_POINT ( 'NONE',  ( 0.000000000000000000, -19.38316218894255627, 61.87375713200982119 ) ) ;
#16953 = CARTESIAN_POINT ( 'NONE',  ( 6.165580000000000283, 0.000000000000000000, 0.000000000000000000 ) ) ;
#16954 = ORIENTED_EDGE ( 'NONE', *, *, #14351, .T. ) ;
#16955 = ORIENTED_EDGE ( 'NONE', *, *, #9604, .T. ) ;
#16956 = DIRECTION ( 'NONE',  ( -1.000000000000000000, 0.000000000000000000, 0.000000000000000000 ) ) ;
#16957 = B_SPLINE_CURVE_WITH_KNOTS ( 'NONE', 3,
 ( #13340, #13542, #10050, #18105, #19987, #13649, #8447, #15029 ),
 .UNSPECIFIED., .F., .F.,
 ( 4, 2, 2, 4 ),
 ( 0.000000000000000000, 0.004499419545982465997, 0.006749129318973705501, 0.008998839091964944137 ),
 .UNSPECIFIED. ) ;
#16958 = EDGE_CURVE ( 'NONE', #20075, #16753, #15238, .T. ) ;
#16959 = DIRECTION ( 'NONE',  ( -1.000000000000000000, -0.000000000000000000, 0.000000000000000000 ) ) ;
#16960 = EDGE_CURVE ( 'NONE', #18276, #7721, #865, .T. ) ;
#16961 = EDGE_CURVE ( 'NONE', #16611, #4158, #6102, .T. ) ;
#16962 = DIRECTION ( 'NONE',  ( 1.000000000000000000, 0.000000000000000000, 0.000000000000000000 ) ) ;
#16963 = CIRCLE ( 'NONE', #19668, 2.649999999999988365 ) ;
#16964 = VECTOR ( 'NONE', #14183, 1000.000000000000000 ) ;
#16965 = CARTESIAN_POINT ( 'NONE',  ( -1.491842756249031510, -7.499999999820660790, -6.400418749819690056 ) ) ;
#16966 = EDGE_CURVE ( 'NONE', #5273, #17663, #20804, .T. ) ;
#16967 = LINE ( 'NONE', #4139, #5077 ) ;
#16968 = CARTESIAN_POINT ( 'NONE',  ( 24.99999999999999645, -30.00000000000000711, 50.99019513592784847 ) ) ;
#16969 = CARTESIAN_POINT ( 'NONE',  ( 19.99999999999999645, -60.40676135667455071, 23.56039007469017221 ) ) ;
#16970 = ORIENTED_EDGE ( 'NONE', *, *, #18571, .T. ) ;
#16971 = CYLINDRICAL_SURFACE ( 'NONE', #16986, 65.24900000006525147 ) ;
#16972 = VERTEX_POINT ( 'NONE', #16046 ) ;
#16973 = CARTESIAN_POINT ( 'NONE',  ( 10.19618095414378800, 15.25966316918061416, 1.081293750180314372 ) ) ;
#16974 = CARTESIAN_POINT ( 'NONE',  ( 10.47959250967882205, -18.77674085041570962, 71.79709706900059984 ) ) ;
#16975 = AXIS2_PLACEMENT_3D ( 'NONE', #17474, #12386, #1271 ) ;
#16976 = EDGE_LOOP ( 'NONE', ( #8407, #13832, #695, #5373 ) ) ;
#16977 = DIRECTION ( 'NONE',  ( 0.000000000000000000, 0.000000000000000000, 1.000000000000000000 ) ) ;
#16978 = EDGE_LOOP ( 'NONE', ( #15973, #11917, #5392, #9344 ) ) ;
#16979 = CARTESIAN_POINT ( 'NONE',  ( 40.00000000000000711, -122.3205080756887639, 80.28096411455982206 ) ) ;
#16980 = FACE_OUTER_BOUND ( 'NONE', #1667, .T. ) ;
#16981 = FACE_OUTER_BOUND ( 'NONE', #14254, .T. ) ;
#16982 = ORIENTED_EDGE ( 'NONE', *, *, #8085, .F. ) ;
#16983 = PLANE ( 'NONE',  #20143 ) ;
#16984 = AXIS2_PLACEMENT_3D ( 'NONE', #2645, #20542, #15553 ) ;
#16985 = EDGE_CURVE ( 'NONE', #5992, #7974, #16153, .T. ) ;
#16986 = AXIS2_PLACEMENT_3D ( 'NONE', #14128, #2570, #5733 ) ;
#16987 = CIRCLE ( 'NONE', #12253, 21.50000000000000000 ) ;
#16988 = DIRECTION ( 'NONE',  ( -0.000000000000000000, -3.469446951953615175E-16, -1.000000000000000000 ) ) ;
#16989 = CARTESIAN_POINT ( 'NONE',  ( -16.62983158437509701, 6.888301784570728614, -10.99448749981968909 ) ) ;
#16990 = LINE ( 'NONE', #5429, #4883 ) ;
#16991 = ADVANCED_FACE ( 'NONE', ( #9783, #3010 ), #17854, .T. ) ;
#16992 = EDGE_CURVE ( 'NONE', #9250, #2396, #1391, .T. ) ;
#16993 = DIRECTION ( 'NONE',  ( -0.000000000000000000, 1.287488025362403787E-15, 1.000000000000000000 ) ) ;
#16994 = CARTESIAN_POINT ( 'NONE',  ( -7.902369978624331104, -7.902369976724401113, -8.248015249352576461 ) ) ;
#16995 = ORIENTED_EDGE ( 'NONE', *, *, #12003, .F. ) ;
#16996 = ADVANCED_FACE ( 'NONE', ( #13072 ), #5014, .T. ) ;
#16997 = DIRECTION ( 'NONE',  ( 1.000000000000000000, -0.000000000000000000, -0.000000000000000000 ) ) ;
#16998 = ORIENTED_EDGE ( 'NONE', *, *, #13621, .T. ) ;
#16999 = AXIS2_PLACEMENT_3D ( 'NONE', #4334, #18753, #10800 ) ;
#17000 = CARTESIAN_POINT ( 'NONE',  ( -9.587454675490699074, -19.24766271911510529, -71.57389447320451836 ) ) ;
#17001 = AXIS2_PLACEMENT_3D ( 'NONE', #3304, #15910, #4579 ) ;
#17002 = VERTEX_POINT ( 'NONE', #16347 ) ;
#17003 = CARTESIAN_POINT ( 'NONE',  ( -18.00000000043041126, -3.580422610670022099, 8.876518750180313333 ) ) ;
#17004 = CIRCLE ( 'NONE', #12637, 27.60000000002759535 ) ;
#17005 = DIRECTION ( 'NONE',  ( -1.000000000000000000, -0.000000000000000000, -0.000000000000000000 ) ) ;
#17006 = CARTESIAN_POINT ( 'NONE',  ( 4.924999999999924327, -8.530350227276771946, -43.00000000000000000 ) ) ;
#17007 = VERTEX_POINT ( 'NONE', #1837 ) ;
#17008 = DIRECTION ( 'NONE',  ( -0.000000000000000000, -0.000000000000000000, -1.000000000000000000 ) ) ;
#17009 = ORIENTED_EDGE ( 'NONE', *, *, #3395, .F. ) ;
#17010 = DIRECTION ( 'NONE',  ( 1.000000000000000000, 0.000000000000000000, 0.000000000000000000 ) ) ;
#17011 = CIRCLE ( 'NONE', #8879, 27.60000000002759890 ) ;
#17012 = ADVANCED_FACE ( 'NONE', ( #8288 ), #6179, .F. ) ;
#17013 = ORIENTED_EDGE ( 'NONE', *, *, #18666, .F. ) ;
#17014 = CARTESIAN_POINT ( 'NONE',  ( 19.99999999999999645, 0.000000000000000000, 72.00000000007199219 ) ) ;
#17015 = EDGE_CURVE ( 'NONE', #15594, #5687, #9630, .T. ) ;
#17016 = CARTESIAN_POINT ( 'NONE',  ( 62.49999999999999289, -40.00000000000000000, 5.000000000000000000 ) ) ;
#17017 = CIRCLE ( 'NONE', #6846, 80.00000000000000000 ) ;
#17018 = AXIS2_PLACEMENT_3D ( 'NONE', #15782, #89, #15887 ) ;
#17019 = VECTOR ( 'NONE', #6562, 1000.000000000000000 ) ;
#17020 = EDGE_CURVE ( 'NONE', #10665, #13515, #17630, .T. ) ;
#17021 = CARTESIAN_POINT ( 'NONE',  ( 0.000000000000000000, 1.178949249685212974, -2.042000000000001148 ) ) ;
#17022 = AXIS2_PLACEMENT_3D ( 'NONE', #13627, #2290, #13734 ) ;
#17023 = CARTESIAN_POINT ( 'NONE',  ( -12.54593441764187745, -8.382925368423274293, -8.705801831158458626 ) ) ;
#17024 = EDGE_LOOP ( 'NONE', ( #11663, #7053, #18462, #15792 ) ) ;
#17025 = LINE ( 'NONE', #8435, #12279 ) ;
#17026 = ORIENTED_EDGE ( 'NONE', *, *, #2976, .F. ) ;
#17027 = CIRCLE ( 'NONE', #13670, 27.60000000002760601 ) ;
#17028 = CARTESIAN_POINT ( 'NONE',  ( -11.45434770231475596, -18.20738947644333550, 77.71966828574345243 ) ) ;
#17029 = AXIS2_PLACEMENT_3D ( 'NONE', #4025, #12193, #10405 ) ;
#17030 = CARTESIAN_POINT ( 'NONE',  ( -12.72792205982779556, 12.72792206288790773, 8.444575000180309488 ) ) ;
#17031 = FACE_OUTER_BOUND ( 'NONE', #18724, .T. ) ;
#17032 = CIRCLE ( 'NONE', #19406, 3.199999999999994404 ) ;
#17033 = CIRCLE ( 'NONE', #7898, 2.700000000000000622 ) ;
#17034 = ORIENTED_EDGE ( 'NONE', *, *, #13240, .F. ) ;
#17035 = CARTESIAN_POINT ( 'NONE',  ( -24.99999999999999645, -97.49621075554985339, -111.6458212409894486 ) ) ;
#17036 = CARTESIAN_POINT ( 'NONE',  ( 7.500000000000000000, 9.184850993605147944E-16, 40.00000000000000000 ) ) ;
#17037 = ORIENTED_EDGE ( 'NONE', *, *, #3979, .T. ) ;
#17038 = CARTESIAN_POINT ( 'NONE',  ( -7.494266837154794914, -21.79755816881963781, -75.89910374996922826 ) ) ;
#17039 = ORIENTED_EDGE ( 'NONE', *, *, #15150, .F. ) ;
#17040 = CARTESIAN_POINT ( 'NONE',  ( 2.870125741905212635, -6.929096494179677101, 2.140987500180307368 ) ) ;
#17041 = CARTESIAN_POINT ( 'NONE',  ( -15.25966316918061416, 10.19618095414378445, -10.69995624981968874 ) ) ;
#17042 = ORIENTED_EDGE ( 'NONE', *, *, #13253, .T. ) ;
#17043 = AXIS2_PLACEMENT_3D ( 'NONE', #6489, #5016, #138 ) ;
#17044 = ORIENTED_EDGE ( 'NONE', *, *, #5799, .F. ) ;
#17045 = DIRECTION ( 'NONE',  ( -1.000000000000000000, 0.000000000000000000, 0.000000000000000000 ) ) ;
#17046 = AXIS2_PLACEMENT_3D ( 'NONE', #1586, #3562, #6740 ) ;
#17047 = CARTESIAN_POINT ( 'NONE',  ( 0.000000000000000000, 0.000000000000000000, 46.00000000000000711 ) ) ;
#17048 = DIRECTION ( 'NONE',  ( -1.000000000000000000, -0.000000000000000000, 0.000000000000000000 ) ) ;
#17049 = CARTESIAN_POINT ( 'NONE',  ( 19.99999999999999645, -65.23577793412343340, -1.313498510942392450 ) ) ;
#17050 = CARTESIAN_POINT ( 'NONE',  ( -18.00000000000000355, 2.163826221265759298E-09, 9.171050000180310136 ) ) ;
#17051 = CIRCLE ( 'NONE', #18756, 2.649999999999993694 ) ;
#17052 = VECTOR ( 'NONE', #13569, 1000.000000000000000 ) ;
#17053 = DIRECTION ( 'NONE',  ( 1.000000000000000000, 0.000000000000000000, 0.000000000000000000 ) ) ;
#17054 = CARTESIAN_POINT ( 'NONE',  ( -7.500000000000007994, 9.015942588607339023E-10, -7.498799999819685702 ) ) ;
#17055 = DIRECTION ( 'NONE',  ( 0.000000000000000000, 0.000000000000000000, 1.000000000000000000 ) ) ;
#17056 = EDGE_CURVE ( 'NONE', #9376, #14238, #16871, .T. ) ;
#17057 = CARTESIAN_POINT ( 'NONE',  ( 11.17563879731704723, -1.343450868547281106E-09, -9.480109750286803916 ) ) ;
#17058 = ADVANCED_FACE ( 'NONE', ( #14969 ), #19732, .F. ) ;
#17059 = AXIS2_PLACEMENT_3D ( 'NONE', #7555, #15723, #16038 ) ;
#17060 = CARTESIAN_POINT ( 'NONE',  ( 19.99999999999999645, 11.98658579560587789, 64.13855129306472236 ) ) ;
#17061 = VECTOR ( 'NONE', #6206, 1000.000000000000000 ) ;
#17062 = EDGE_LOOP ( 'NONE', ( #12188, #14132, #11684, #12838 ) ) ;
#17063 = DIRECTION ( 'NONE',  ( -1.000000000000000000, 0.000000000000000000, 0.000000000000000000 ) ) ;
#17064 = CARTESIAN_POINT ( 'NONE',  ( -3.580422610670018546, 18.00000000043041126, -7.617231249819687022 ) ) ;
#17065 = CARTESIAN_POINT ( 'NONE',  ( 30.00000000000000000, -49.99999999999999289, -71.93747284969079203 ) ) ;
#17066 = CIRCLE ( 'NONE', #11643, 27.60000000002759535 ) ;
#17067 = VERTEX_POINT ( 'NONE', #6902 ) ;
#17068 = LINE ( 'NONE', #7738, #20709 ) ;
#17069 = ORIENTED_EDGE ( 'NONE', *, *, #11837, .F. ) ;
#17070 = CIRCLE ( 'NONE', #15025, 17.50000000000000355 ) ;
#17071 = CARTESIAN_POINT ( 'NONE',  ( 19.99999999999999645, 31.98952867950403345, -56.39803944231551469 ) ) ;
#17072 = CARTESIAN_POINT ( 'NONE',  ( 34.33484195354434831, -26.68654532909942745, -68.63850682271649362 ) ) ;
#17073 = EDGE_LOOP ( 'NONE', ( #8526, #10773 ) ) ;
#17074 = VERTEX_POINT ( 'NONE', #5316 ) ;
#17075 = DIRECTION ( 'NONE',  ( -0.000000000000000000, 0.000000000000000000, -1.000000000000000000 ) ) ;
#17076 = AXIS2_PLACEMENT_3D ( 'NONE', #20594, #3004, #14356 ) ;
#17077 = PRESENTATION_STYLE_ASSIGNMENT (( #10617 ) ) ;
#17078 = CARTESIAN_POINT ( 'NONE',  ( 17.99999999999999645, -2.163824016901520184E-09, 21.40395000018031268 ) ) ;
#17079 = CYLINDRICAL_SURFACE ( 'NONE', #5211, 2.649999999999999467 ) ;
#17080 = VECTOR ( 'NONE', #10491, 1000.000000000000000 ) ;
#17081 = CARTESIAN_POINT ( 'NONE',  ( 6.929096493489624642, -2.870125743571141363, -8.462137499819689879 ) ) ;
#17082 = EDGE_CURVE ( 'NONE', #10203, #16753, #15175, .T. ) ;
#17083 = SURFACE_STYLE_FILL_AREA ( #1196 ) ;
#17084 = DIRECTION ( 'NONE',  ( 0.000000000000000000, 0.5195839500354290097, 0.8544194045464913456 ) ) ;
#17085 = CARTESIAN_POINT ( 'NONE',  ( 4.000000000000004441, 0.7862748000878170274, -5.565527722372433317 ) ) ;
#17086 = LINE ( 'NONE', #15494, #1230 ) ;
#17087 = ORIENTED_EDGE ( 'NONE', *, *, #12868, .F. ) ;
#17088 = CARTESIAN_POINT ( 'NONE',  ( 21.00000000000000355, 0.000000000000000000, 2.055000000000000160 ) ) ;
#17089 = EDGE_LOOP ( 'NONE', ( #1523, #6299, #4369, #6847 ) ) ;
#17090 = CARTESIAN_POINT ( 'NONE',  ( 6.888301784570728614, 16.62983158437510056, 10.21176250018031517 ) ) ;
#17091 = CARTESIAN_POINT ( 'NONE',  ( -21.45900938229203447, -1.326995226329893862, 84.99999999999998579 ) ) ;
#17092 = ORIENTED_EDGE ( 'NONE', *, *, #17213, .F. ) ;
#17093 = ADVANCED_FACE ( 'NONE', ( #16654 ), #2141, .F. ) ;
#17094 = CARTESIAN_POINT ( 'NONE',  ( 19.99999999999999645, 0.000000000000000000, 0.000000000000000000 ) ) ;
#17095 = ORIENTED_EDGE ( 'NONE', *, *, #4820, .T. ) ;
#17096 = LINE ( 'NONE', #2579, #360 ) ;
#17097 = FACE_BOUND ( 'NONE', #2997, .T. ) ;
#17098 = DIRECTION ( 'NONE',  ( 1.000000000000000000, 0.000000000000000000, 0.000000000000000000 ) ) ;
#17099 = ORIENTED_EDGE ( 'NONE', *, *, #5172, .F. ) ;
#17100 = FACE_OUTER_BOUND ( 'NONE', #17286, .T. ) ;
#17101 = AXIS2_PLACEMENT_3D ( 'NONE', #8313, #5341, #14787 ) ;
#17102 = DIRECTION ( 'NONE',  ( 0.000000000000000000, 0.000000000000000000, -1.000000000000000000 ) ) ;
#17103 = CARTESIAN_POINT ( 'NONE',  ( -15.25966317163202923, -10.19618095047497874, -12.46714374981969264 ) ) ;
#17104 = DIRECTION ( 'NONE',  ( -0.000000000000000000, -3.469446951953614682E-16, -1.000000000000000000 ) ) ;
#17105 = EDGE_CURVE ( 'NONE', #18656, #12982, #557, .T. ) ;
#17106 = DIRECTION ( 'NONE',  ( 0.000000000000000000, 0.000000000000000000, 1.000000000000000000 ) ) ;
#17107 = CARTESIAN_POINT ( 'NONE',  ( 10.32494394809439875, 4.276731812588567827, -12.37145274935257255 ) ) ;
#17108 = EDGE_LOOP ( 'NONE', ( #20617, #15547 ) ) ;
#17109 =( NAMED_UNIT ( * ) PLANE_ANGLE_UNIT ( ) SI_UNIT ( $, .RADIAN. ) );
#17110 = CARTESIAN_POINT ( 'NONE',  ( 3.600000000000054712, 10.82531754730546147, 43.00000000000000000 ) ) ;
#17111 = VERTEX_POINT ( 'NONE', #13488 ) ;
#17112 = CARTESIAN_POINT ( 'NONE',  ( 13.23800900960920401, -16.95692081615698044, -72.71034110640576387 ) ) ;
#17113 = LINE ( 'NONE', #17324, #4161 ) ;
#17114 = VECTOR ( 'NONE', #14146, 1000.000000000000000 ) ;
#17115 = ORIENTED_EDGE ( 'NONE', *, *, #4027, .T. ) ;
#17116 = CARTESIAN_POINT ( 'NONE',  ( 16.62983158603122291, 6.888301780572502864, -14.98051249981969058 ) ) ;
#17117 = FACE_OUTER_BOUND ( 'NONE', #17760, .T. ) ;
#17118 = DIRECTION ( 'NONE',  ( 0.000000000000000000, 0.000000000000000000, 1.000000000000000000 ) ) ;
#17119 = ORIENTED_EDGE ( 'NONE', *, *, #19834, .F. ) ;
#17120 = EDGE_CURVE ( 'NONE', #7974, #880, #2717, .T. ) ;
#17121 = DIRECTION ( 'NONE',  ( -1.648349939164583742E-16, 1.000000000000000000, 0.000000000000000000 ) ) ;
#17122 = ORIENTED_EDGE ( 'NONE', *, *, #9082, .T. ) ;
#17123 = FACE_OUTER_BOUND ( 'NONE', #3202, .T. ) ;
#17124 = ADVANCED_FACE ( 'NONE', ( #13276 ), #16448, .T. ) ;
#17125 = EDGE_LOOP ( 'NONE', ( #10716, #1520 ) ) ;
#17126 = VECTOR ( 'NONE', #1366, 1000.000000000000000 ) ;
#17127 = EDGE_CURVE ( 'NONE', #17270, #20602, #14912, .T. ) ;
#17128 = EDGE_CURVE ( 'NONE', #1644, #18621, #20315, .T. ) ;
#17129 = DIRECTION ( 'NONE',  ( 0.000000000000000000, 0.000000000000000000, 1.000000000000000000 ) ) ;
#17130 = PRODUCT_DEFINITION ( 'UNKNOWN', '', #16754, #20224 ) ;
#17131 = CIRCLE ( 'NONE', #19827, 21.50000000000000000 ) ;
#17132 = FACE_OUTER_BOUND ( 'NONE', #3325, .T. ) ;
#17133 = CARTESIAN_POINT ( 'NONE',  ( -14.79893867793684059, -2.943691925285399691, -8.116739331158456139 ) ) ;
#17134 = ORIENTED_EDGE ( 'NONE', *, *, #20714, .F. ) ;
#17135 = CARTESIAN_POINT ( 'NONE',  ( -4.000000000000000000, -0.7779732554280797130, -5.566455648918322119 ) ) ;
#17136 = ORIENTED_EDGE ( 'NONE', *, *, #8027, .F. ) ;
#17137 = ADVANCED_FACE ( 'NONE', ( #18988 ), #10507, .F. ) ;
#17138 = CARTESIAN_POINT ( 'NONE',  ( 0.000000000000000000, 14.55863677812122425, 63.60407295269110506 ) ) ;
#17139 = EDGE_CURVE ( 'NONE', #2408, #1189, #7642, .T. ) ;
#17140 = CARTESIAN_POINT ( 'NONE',  ( 18.00000000043040771, 3.580422610670018546, 2.259418750180309576 ) ) ;
#17141 = PLANE ( 'NONE',  #10548 ) ;
#17142 = DIRECTION ( 'NONE',  ( 0.000000000000000000, 0.000000000000000000, -1.000000000000000000 ) ) ;
#17143 = VECTOR ( 'NONE', #16531, 1000.000000000000000 ) ;
#17144 = VERTEX_POINT ( 'NONE', #5623 ) ;
#17145 = ADVANCED_FACE ( 'NONE', ( #4461 ), #10929, .T. ) ;
#17146 = DIRECTION ( 'NONE',  ( -1.000000000000000000, -0.000000000000000000, -0.000000000000000000 ) ) ;
#17147 = DIRECTION ( 'NONE',  ( -0.000000000000000000, -1.000000000000000000, -0.000000000000000000 ) ) ;
#17148 = ORIENTED_EDGE ( 'NONE', *, *, #8280, .T. ) ;
#17149 = CARTESIAN_POINT ( 'NONE',  ( 10.34366295437100014, -20.54632100680313656, -76.49602251636484596 ) ) ;
#17150 = CARTESIAN_POINT ( 'NONE',  ( -7.500000000000002665, -1.491842754878805355, 4.791768750087786799 ) ) ;
#17151 = EDGE_CURVE ( 'NONE', #9587, #8741, #13903, .T. ) ;
#17152 = CARTESIAN_POINT ( 'NONE',  ( 18.00000000043040771, 3.580422610670018546, -7.165581249819689802 ) ) ;
#17153 = CIRCLE ( 'NONE', #3940, 2.649999999999993694 ) ;
#17154 = ORIENTED_EDGE ( 'NONE', *, *, #166, .F. ) ;
#17155 = EDGE_CURVE ( 'NONE', #3220, #3544, #17406, .T. ) ;
#17156 = VERTEX_POINT ( 'NONE', #15698 ) ;
#17157 = DIRECTION ( 'NONE',  ( 1.000000000000000000, -0.000000000000000000, -0.000000000000000000 ) ) ;
#17158 = CIRCLE ( 'NONE', #15457, 72.00000000007199219 ) ;
#17159 = DIRECTION ( 'NONE',  ( 0.000000000000000000, 0.000000000000000000, -1.000000000000000000 ) ) ;
#17160 = AXIS2_PLACEMENT_3D ( 'NONE', #8359, #17814, #16215 ) ;
#17161 = DIRECTION ( 'NONE',  ( -1.000000000000000000, -0.000000000000000000, 0.000000000000000000 ) ) ;
#17162 = DIRECTION ( 'NONE',  ( -1.000000000000000000, -0.000000000000000000, -0.000000000000000000 ) ) ;
#17163 = CARTESIAN_POINT ( 'NONE',  ( -2.163827323447878648E-09, -18.00000000000000355, 6.814800000180309958 ) ) ;
#17164 = AXIS2_PLACEMENT_3D ( 'NONE', #9091, #5906, #6214 ) ;
#17165 =( GEOMETRIC_REPRESENTATION_CONTEXT ( 3 ) GLOBAL_UNCERTAINTY_ASSIGNED_CONTEXT ( ( #6869 ) ) GLOBAL_UNIT_ASSIGNED_CONTEXT ( ( #20342, #18887, #13800 ) ) REPRESENTATION_CONTEXT ( 'NONE', 'WORKASPACE' ) );
#17166 = CARTESIAN_POINT ( 'NONE',  ( -4.248408730893249441, -6.358192987158595599, -18.39645624981969263 ) ) ;
#17167 = ORIENTED_EDGE ( 'NONE', *, *, #4652, .F. ) ;
#17168 = CARTESIAN_POINT ( 'NONE',  ( 19.99999999999999645, 0.000000000000000000, 0.000000000000000000 ) ) ;
#17169 = EDGE_CURVE ( 'NONE', #2557, #10176, #11219, .T. ) ;
#17170 = CARTESIAN_POINT ( 'NONE',  ( 2.222972768810837163, -11.17563879758427525, -26.26839100028680107 ) ) ;
#17171 = VECTOR ( 'NONE', #5495, 1000.000000000000000 ) ;
#17172 = DIRECTION ( 'NONE',  ( 0.000000000000000000, 0.000000000000000000, 1.000000000000000000 ) ) ;
#17173 = VERTEX_POINT ( 'NONE', #18667 ) ;
#17174 = CARTESIAN_POINT ( 'NONE',  ( 0.000000000000000000, 5.762283366692075859, -64.99406197038663890 ) ) ;
#17175 = CIRCLE ( 'NONE', #20884, 10.00000000000000178 ) ;
#17176 = CARTESIAN_POINT ( 'NONE',  ( -17.50000000000000355, 0.000000000000000000, -40.00000000000000000 ) ) ;
#17177 = DIRECTION ( 'NONE',  ( -1.000000000000000000, 0.000000000000000000, 0.000000000000000000 ) ) ;
#17178 = VERTEX_POINT ( 'NONE', #20467 ) ;
#17179 = CYLINDRICAL_SURFACE ( 'NONE', #14632, 2.099999999999997868 ) ;
#17180 = VECTOR ( 'NONE', #19170, 1000.000000000000000 ) ;
#17181 = ORIENTED_EDGE ( 'NONE', *, *, #5149, .F. ) ;
#17182 = DIRECTION ( 'NONE',  ( -0.5000000000000051070, 1.060575238724903217E-16, -0.8660254037844355990 ) ) ;
#17183 = DIRECTION ( 'NONE',  ( 0.000000000000000000, 0.000000000000000000, 1.000000000000000000 ) ) ;
#17184 = B_SPLINE_CURVE_WITH_KNOTS ( 'NONE', 3,
 ( #2092, #18524, #19986, #3987, #2196, #5469, #18211, #2404, #12155, #7273, #5371, #13541, #7061, #8863, #3771, #3675, #18622, #5269, #1997, #11839, #10049, #8548, #18306, #10254 ),
 .UNSPECIFIED., .F., .F.,
 ( 4, 2, 2, 2, 2, 2, 2, 2, 2, 2, 2, 4 ),
 ( 1.430489624538199204E-17, 0.002868008191885854877, 0.005736016383771695010, 0.007170020479714604884, 0.008604024575657518228, 0.01147203276754338135, 0.01290603686348630076, 0.01434004095942921671, 0.01720804915131499135, 0.02007605734320076774, 0.02151006143914363511, 0.02294406553508650942 ),
 .UNSPECIFIED. ) ;
#17185 = AXIS2_PLACEMENT_3D ( 'NONE', #8372, #3082, #4004 ) ;
#17186 = ORIENTED_EDGE ( 'NONE', *, *, #1340, .T. ) ;
#17187 = VERTEX_POINT ( 'NONE', #7208 ) ;
#17188 = DIRECTION ( 'NONE',  ( 0.000000000000000000, 0.000000000000000000, 1.000000000000000000 ) ) ;
#17189 = EDGE_CURVE ( 'NONE', #11808, #11920, #20351, .T. ) ;
#17190 = AXIS2_PLACEMENT_3D ( 'NONE', #15542, #17147, #14079 ) ;
#17191 = SURFACE_STYLE_USAGE ( .BOTH. , #2559 ) ;
#17192 = CARTESIAN_POINT ( 'NONE',  ( 19.99999999999999645, 63.05226888949891162, 15.11556105343481882 ) ) ;
#17193 = CIRCLE ( 'NONE', #20572, 27.60000000002759535 ) ;
#17194 = DIRECTION ( 'NONE',  ( -0.000000000000000000, -0.000000000000000000, 1.000000000000000000 ) ) ;
#17195 = VECTOR ( 'NONE', #8776, 1000.000000000000000 ) ;
#17196 = CARTESIAN_POINT ( 'NONE',  ( 1.491842756249028845, 7.499999999820661678, -20.53791874981969556 ) ) ;
#17197 =( NAMED_UNIT ( * ) SI_UNIT ( $, .STERADIAN. ) SOLID_ANGLE_UNIT ( ) );
#17198 = DIRECTION ( 'NONE',  ( -0.000000000000000000, -0.000000000000000000, 1.000000000000000000 ) ) ;
#17199 = DIRECTION ( 'NONE',  ( 0.000000000000000000, -8.673617379884034239E-17, -1.000000000000000000 ) ) ;
#17200 = ORIENTED_EDGE ( 'NONE', *, *, #13150, .T. ) ;
#17201 = CARTESIAN_POINT ( 'NONE',  ( 19.99999999999999645, -11.98658579560631843, 64.13855129306463709 ) ) ;
#17202 = ORIENTED_EDGE ( 'NONE', *, *, #13605, .T. ) ;
#17203 = CARTESIAN_POINT ( 'NONE',  ( -3.580422610670018546, 18.00000000043041126, -18.94683124981968803 ) ) ;
#17204 = DIRECTION ( 'NONE',  ( -1.000000000000000000, 0.000000000000000000, 0.000000000000000000 ) ) ;
#17205 = ORIENTED_EDGE ( 'NONE', *, *, #8071, .T. ) ;
#17206 = LINE ( 'NONE', #6161, #7915 ) ;
#17207 = ORIENTED_EDGE ( 'NONE', *, *, #12037, .F. ) ;
#17208 = DIRECTION ( 'NONE',  ( -1.000000000000000000, 0.000000000000000000, 0.000000000000000000 ) ) ;
#17209 = CARTESIAN_POINT ( 'NONE',  ( 52.50000000000000000, -40.00000000000000000, 5.000000000000000000 ) ) ;
#17210 = CARTESIAN_POINT ( 'NONE',  ( 11.50000000000000000, 0.000000000000000000, 68.00000000000000000 ) ) ;
#17211 = ORIENTED_EDGE ( 'NONE', *, *, #504, .F. ) ;
#17212 = CARTESIAN_POINT ( 'NONE',  ( 5.303300858261588147, -5.303300859536636658, -20.45817499981968624 ) ) ;
#17213 = EDGE_CURVE ( 'NONE', #20537, #18745, #9235, .T. ) ;
#17214 = DIRECTION ( 'NONE',  ( -1.000000000000000000, 0.000000000000000000, -0.000000000000000000 ) ) ;
#17215 = CARTESIAN_POINT ( 'NONE',  ( 3.580422610670019878, -18.00000000043040771, -23.65933124981969016 ) ) ;
#17216 = DIRECTION ( 'NONE',  ( -0.000000000000000000, -0.000000000000000000, 1.000000000000000000 ) ) ;
#17217 = CARTESIAN_POINT ( 'NONE',  ( 6.358192987158592047, -4.248408730893246776, 10.68239375018030834 ) ) ;
#17218 = ORIENTED_EDGE ( 'NONE', *, *, #18663, .F. ) ;
#17219 = FILL_AREA_STYLE ('',( #12343 ) ) ;
#17220 = MANIFOLD_SOLID_BREP ( 'Extrude-Thin1', #17363 ) ;
#17221 = DIRECTION ( 'NONE',  ( 0.000000000000000000, 0.000000000000000000, -1.000000000000000000 ) ) ;
#17222 = VERTEX_POINT ( 'NONE', #6051 ) ;
#17223 = CIRCLE ( 'NONE', #19909, 17.50000000000000355 ) ;
#17224 = PLANE ( 'NONE',  #4868 ) ;
#17225 = CARTESIAN_POINT ( 'NONE',  ( 17.00000000000000000, 0.000000000000000000, 2.055000000000000160 ) ) ;
#17226 = ORIENTED_EDGE ( 'NONE', *, *, #10727, .T. ) ;
#17227 = CARTESIAN_POINT ( 'NONE',  ( 2.163825119083639534E-09, 18.00000000000000000, -7.322699999819687555 ) ) ;
#17228 = DIRECTION ( 'NONE',  ( 0.000000000000000000, 0.000000000000000000, -1.000000000000000000 ) ) ;
#17229 = CARTESIAN_POINT ( 'NONE',  ( -2.099999999999999645, 2.571758278209440971E-16, -0.2800830152838832965 ) ) ;
#17230 = VERTEX_POINT ( 'NONE', #2565 ) ;
#17231 = DIRECTION ( 'NONE',  ( -1.000000000000000000, 0.000000000000000000, 0.000000000000000000 ) ) ;
#17232 = ORIENTED_EDGE ( 'NONE', *, *, #9866, .F. ) ;
#17233 = CARTESIAN_POINT ( 'NONE',  ( 2.870125743571140475, 6.929096493489632635, 14.29651250018031661 ) ) ;
#17234 = ORIENTED_EDGE ( 'NONE', *, *, #12609, .T. ) ;
#17235 = DIRECTION ( 'NONE',  ( 0.000000000000000000, 0.000000000000000000, 1.000000000000000000 ) ) ;
#17236 = CARTESIAN_POINT ( 'NONE',  ( -62.49999999999999289, -130.0000000000000000, 5.000000000000000000 ) ) ;
#17237 = CONTEXT_DEPENDENT_SHAPE_REPRESENTATION ( #5201, #18473 ) ;
#17238 = CARTESIAN_POINT ( 'NONE',  ( 5.663308650141532397, 13.67243654642775574, 4.548104418841546703 ) ) ;
#17239 = ADVANCED_FACE ( 'NONE', ( #5945 ), #2671, .T. ) ;
#17240 = ORIENTED_EDGE ( 'NONE', *, *, #3710, .T. ) ;
#17241 = ADVANCED_FACE ( 'NONE', ( #2449 ), #7530, .F. ) ;
#17242 = DIRECTION ( 'NONE',  ( -1.000000000000000000, 0.000000000000000000, 0.000000000000000000 ) ) ;
#17243 = VERTEX_POINT ( 'NONE', #13806 ) ;
#17244 = CARTESIAN_POINT ( 'NONE',  ( -10.86880604054440269, -18.56337176816380108, 77.52347650517093314 ) ) ;
#17245 = CARTESIAN_POINT ( 'NONE',  ( 15.25966317163202568, 10.19618095047498230, 1.670356250180308422 ) ) ;
#17246 = CARTESIAN_POINT ( 'NONE',  ( 49.35000000000000142, -99.99999999999998579, 0.000000000000000000 ) ) ;
#17247 = DIRECTION ( 'NONE',  ( 1.000000000000000000, 0.000000000000000000, 0.000000000000000000 ) ) ;
#17248 = EDGE_CURVE ( 'NONE', #1656, #11513, #8070, .T. ) ;
#17249 = ORIENTED_EDGE ( 'NONE', *, *, #20228, .F. ) ;
#17250 = LINE ( 'NONE', #8979, #19528 ) ;
#17251 = CARTESIAN_POINT ( 'NONE',  ( 0.000000000000000000, 0.000000000000000000, 46.00000000000000711 ) ) ;
#17252 = APPLICATION_CONTEXT ( 'automotive_design' ) ;
#17253 = ORIENTED_EDGE ( 'NONE', *, *, #12765, .T. ) ;
#17254 = CARTESIAN_POINT ( 'NONE',  ( -21.45900938229203447, -1.326995226329893862, 84.99999999999998579 ) ) ;
#17255 = CARTESIAN_POINT ( 'NONE',  ( 56.98610214956098474, -164.9999999999999716, -84.54208835637706443 ) ) ;
#17256 = CARTESIAN_POINT ( 'NONE',  ( 18.00000000043040771, 3.580422610670018546, -16.59058124981969229 ) ) ;
#17257 = ORIENTED_EDGE ( 'NONE', *, *, #5770, .F. ) ;
#17258 = CYLINDRICAL_SURFACE ( 'NONE', #18515, 27.60000000002759890 ) ;
#17259 = EDGE_CURVE ( 'NONE', #14491, #18356, #18325, .T. ) ;
#17260 = CYLINDRICAL_SURFACE ( 'NONE', #12604, 2.099999999999997868 ) ;
#17261 = DIRECTION ( 'NONE',  ( -0.000000000000000000, -0.000000000000000000, -1.000000000000000000 ) ) ;
#17262 = FACE_OUTER_BOUND ( 'NONE', #18822, .T. ) ;
#17263 = DIRECTION ( 'NONE',  ( 6.982962677686266711E-15, 0.000000000000000000, -1.000000000000000000 ) ) ;
#17264 = CARTESIAN_POINT ( 'NONE',  ( 15.25966317163203101, 10.19618095047498585, 12.99995625018031120 ) ) ;
#17265 = EDGE_CURVE ( 'NONE', #5277, #6801, #8494, .T. ) ;
#17266 = AXIS2_PLACEMENT_3D ( 'NONE', #2488, #8948, #15413 ) ;
#17267 = PRODUCT_DEFINITION_CONTEXT ( 'detailed design', #18609, 'design' ) ;
#17268 = EDGE_CURVE ( 'NONE', #4973, #17868, #17610, .T. ) ;
#17269 = CARTESIAN_POINT ( 'NONE',  ( -4.248408729364580694, 6.358192988180020322, -15.45114374981968730 ) ) ;
#17270 = VERTEX_POINT ( 'NONE', #14438 ) ;
#17271 = CARTESIAN_POINT ( 'NONE',  ( 1.040949779275250179E-14, -85.00000000000000000, 5.000000000000000000 ) ) ;
#17272 = CARTESIAN_POINT ( 'NONE',  ( -14.79893867793683349, -2.943691925285398359, 5.115176831519075762 ) ) ;
#17273 = ADVANCED_FACE ( 'NONE', ( #14539 ), #20885, .F. ) ;
#17274 = DIRECTION ( 'NONE',  ( 0.000000000000000000, -1.000000000000000000, 1.224646799147355426E-16 ) ) ;
#17275 = VERTEX_POINT ( 'NONE', #12847 ) ;
#17276 = DIRECTION ( 'NONE',  ( -0.000000000000000000, -0.000000000000000000, 1.000000000000000000 ) ) ;
#17277 = CARTESIAN_POINT ( 'NONE',  ( 17.99999999956958163, -3.580422614997676334, -23.52191874981969377 ) ) ;
#17278 = CYLINDRICAL_SURFACE ( 'NONE', #5655, 2.649999999999992806 ) ;
#17279 = VERTEX_POINT ( 'NONE', #14223 ) ;
#17280 = CARTESIAN_POINT ( 'NONE',  ( -15.15000000000000568, -3.245314017740485469E-16, -43.00000000000000000 ) ) ;
#17281 = ORIENTED_EDGE ( 'NONE', *, *, #15068, .F. ) ;
#17282 = EDGE_CURVE ( 'NONE', #16924, #14502, #15279, .T. ) ;
#17283 = DIRECTION ( 'NONE',  ( -1.000000000000000000, 0.000000000000000000, 0.000000000000000000 ) ) ;
#17284 = DIRECTION ( 'NONE',  ( 1.000000000000000000, -0.000000000000000000, -0.000000000000000000 ) ) ;
#17285 = ORIENTED_EDGE ( 'NONE', *, *, #8593, .T. ) ;
#17286 = EDGE_LOOP ( 'NONE', ( #14249, #16706, #7220, #16561 ) ) ;
#17287 = CARTESIAN_POINT ( 'NONE',  ( 39.24980374687644513, -121.8707082894959939, -79.92871449913415915 ) ) ;
#17288 = EDGE_CURVE ( 'NONE', #10258, #11637, #3108, .T. ) ;
#17289 = AXIS2_PLACEMENT_3D ( 'NONE', #20138, #1380, #19270 ) ;
#17290 = DIRECTION ( 'NONE',  ( -0.000000000000000000, -0.000000000000000000, -1.000000000000000000 ) ) ;
#17291 = EDGE_CURVE ( 'NONE', #18936, #5467, #51, .T. ) ;
#17292 = CARTESIAN_POINT ( 'NONE',  ( 7.574999999999881162, -13.12028486733431976, -40.00000000000000000 ) ) ;
#17293 = CARTESIAN_POINT ( 'NONE',  ( 2.870125741905211747, -6.929096494179675325, -16.70901249981968917 ) ) ;
#17294 = VECTOR ( 'NONE', #5436, 1000.000000000000114 ) ;
#17295 = DIRECTION ( 'NONE',  ( 1.000000000000000000, 0.000000000000000000, 0.000000000000000000 ) ) ;
#17296 = CARTESIAN_POINT ( 'NONE',  ( 0.000000000000000000, 0.000000000000000000, 40.00000000000000000 ) ) ;
#17297 = CARTESIAN_POINT ( 'NONE',  ( -6.999999999999997335, 11.17999999999999972, 0.000000000000000000 ) ) ;
#17298 = ORIENTED_EDGE ( 'NONE', *, *, #1907, .T. ) ;
#17299 = EDGE_CURVE ( 'NONE', #8326, #306, #11353, .T. ) ;
#17300 = LINE ( 'NONE', #9242, #60 ) ;
#17301 = VERTEX_POINT ( 'NONE', #6459 ) ;
#17302 = CARTESIAN_POINT ( 'NONE',  ( 3.580422610670020322, -18.00000000043041126, -14.23433124981968412 ) ) ;
#17303 = CARTESIAN_POINT ( 'NONE',  ( 6.177131623262577698, 0.000000000000000000, 0.000000000000000000 ) ) ;
#17304 = VECTOR ( 'NONE', #6499, 1000.000000000000000 ) ;
#17305 = ORIENTED_EDGE ( 'NONE', *, *, #4188, .T. ) ;
#17306 = DIRECTION ( 'NONE',  ( -1.000000000000000000, 0.000000000000000000, 0.000000000000000000 ) ) ;
#17307 = VERTEX_POINT ( 'NONE', #19101 ) ;
#17308 = CARTESIAN_POINT ( 'NONE',  ( 2.870125741905212635, -6.929096494179677101, -7.284012499819692010 ) ) ;
#17309 = PLANE ( 'NONE',  #19546 ) ;
#17310 = DIRECTION ( 'NONE',  ( 0.000000000000000000, 0.000000000000000000, 1.000000000000000000 ) ) ;
#17311 = ORIENTED_EDGE ( 'NONE', *, *, #6796, .F. ) ;
#17312 = CARTESIAN_POINT ( 'NONE',  ( -39.99999999999999289, -30.00000000000000000, -120.0000000000000142 ) ) ;
#17313 = LINE ( 'NONE', #17428, #11061 ) ;
#17314 = CARTESIAN_POINT ( 'NONE',  ( 0.000000000000000000, 0.000000000000000000, 0.000000000000000000 ) ) ;
#17315 = CARTESIAN_POINT ( 'NONE',  ( -54.64999999999999858, -99.99999999999998579, 5.000000000000000000 ) ) ;
#17316 = CARTESIAN_POINT ( 'NONE',  ( 0.2500000000000002220, 4.898587196589412829E-16, -4.000000000000000000 ) ) ;
#17317 = AXIS2_PLACEMENT_3D ( 'NONE', #4123, #2230, #8900 ) ;
#17318 = ORIENTED_EDGE ( 'NONE', *, *, #2110, .F. ) ;
#17319 = LINE ( 'NONE', #6072, #7621 ) ;
#17320 = CYLINDRICAL_SURFACE ( 'NONE', #16261, 65.24900000006525147 ) ;
#17321 = EDGE_LOOP ( 'NONE', ( #16388, #12096 ) ) ;
#17322 = AXIS2_PLACEMENT_3D ( 'NONE', #2534, #2644, #18955 ) ;
#17323 = DIRECTION ( 'NONE',  ( 0.000000000000000000, 0.000000000000000000, -1.000000000000000000 ) ) ;
#17324 = CARTESIAN_POINT ( 'NONE',  ( 30.00000000000000000, -110.0000000000000142, -1.426443885047873890E-14 ) ) ;
#17325 = EDGE_CURVE ( 'NONE', #9479, #15726, #11889, .T. ) ;
#17326 = ORIENTED_EDGE ( 'NONE', *, *, #537, .T. ) ;
#17327 = ADVANCED_FACE ( 'NONE', ( #2875 ), #5121, .T. ) ;
#17328 = CARTESIAN_POINT ( 'NONE',  ( -12.72792206288791128, -12.72792205982779912, -20.28207499981969164 ) ) ;
#17329 = CYLINDRICAL_SURFACE ( 'NONE', #14451, 2.649999999999999467 ) ;
#17330 = FACE_OUTER_BOUND ( 'NONE', #18517, .T. ) ;
#17331 = AXIS2_PLACEMENT_3D ( 'NONE', #18635, #4100, #5586 ) ;
#17332 = ORIENTED_EDGE ( 'NONE', *, *, #16419, .T. ) ;
#17333 = CIRCLE ( 'NONE', #10559, 65.24900000006525147 ) ;
#17334 = DIRECTION ( 'NONE',  ( 0.000000000000000000, -0.9790840876823206917, -0.2034560130526446298 ) ) ;
#17335 = EDGE_LOOP ( 'NONE', ( #9482, #4446, #11360, #5716 ) ) ;
#17336 = FACE_OUTER_BOUND ( 'NONE', #13450, .T. ) ;
#17337 = CIRCLE ( 'NONE', #8183, 65.24900000006526568 ) ;
#17338 = EDGE_LOOP ( 'NONE', ( #3449, #6720, #17042, #4397 ) ) ;
#17339 = AXIS2_PLACEMENT_3D ( 'NONE', #20847, #15874, #1371 ) ;
#17340 = CARTESIAN_POINT ( 'NONE',  ( -25.00000000000000000, -30.00000000000000711, 58.09475019311124555 ) ) ;
#17341 = LINE ( 'NONE', #19337, #5505 ) ;
#17342 = CARTESIAN_POINT ( 'NONE',  ( -12.54593441562641054, 8.382925371439629458, 2.486385668841545993 ) ) ;
#17343 = CIRCLE ( 'NONE', #18702, 27.60000000002759535 ) ;
#17345 = VERTEX_POINT ( 'NONE', #6151 ) ;
#17344 = AXIS2_PLACEMENT_3D ( 'NONE', #19813, #18233, #6983 ) ;
#17346 = CYLINDRICAL_SURFACE ( 'NONE', #16056, 72.00000000007199219 ) ;
#17347 = VECTOR ( 'NONE', #196, 1000.000000000000000 ) ;
#17348 = ORIENTED_EDGE ( 'NONE', *, *, #4704, .T. ) ;
#17349 = CARTESIAN_POINT ( 'NONE',  ( -7.500000000000004441, 9.706494107352906755E-15, -23.18869999999769860 ) ) ;
#17350 = CARTESIAN_POINT ( 'NONE',  ( 3.580422610670019878, -18.00000000043040771, 14.04066875018031091 ) ) ;
#17351 = DIRECTION ( 'NONE',  ( -1.000000000000000000, 0.000000000000000000, 0.000000000000000000 ) ) ;
#17352 = DIRECTION ( 'NONE',  ( -0.000000000000000000, -0.000000000000000000, 1.000000000000000000 ) ) ;
#17353 = VERTEX_POINT ( 'NONE', #12639 ) ;
#17354 = CARTESIAN_POINT ( 'NONE',  ( 30.00000000000000000, -30.00000000000000711, 58.09475019311124555 ) ) ;
#17355 = FACE_OUTER_BOUND ( 'NONE', #1065, .T. ) ;
#17356 = VERTEX_POINT ( 'NONE', #4573 ) ;
#17357 = AXIS2_PLACEMENT_3D ( 'NONE', #16811, #2393, #5894 ) ;
#17358 = EDGE_CURVE ( 'NONE', #13364, #16482, #2763, .T. ) ;
#17359 = CYLINDRICAL_SURFACE ( 'NONE', #3133, 80.00000000000000000 ) ;
#17360 = AXIS2_PLACEMENT_3D ( 'NONE', #4503, #7785, #9168 ) ;
#17361 = LINE ( 'NONE', #9414, #20352 ) ;
#17362 = CARTESIAN_POINT ( 'NONE',  ( 3.580422614997667896, 17.99999999956958163, -18.35776874981969442 ) ) ;
#17363 = CLOSED_SHELL ( 'NONE', ( #19775, #5710, #10141, #8263, #15964, #546, #10113, #4298, #14013, #20274, #1974, #8203, #14570, #20575, #6308, #20381, #10774, #8089, #10788, #2685, #20646, #9486, #8696, #13075, #14909, #13259 ) ) ;
#17364 = AXIS2_PLACEMENT_3D ( 'NONE', #3248, #19052, #17468 ) ;
#17365 = EDGE_LOOP ( 'NONE', ( #19403, #11104, #15667, #12081 ) ) ;
#17366 = DIRECTION ( 'NONE',  ( -1.000000000000000000, 0.000000000000000000, 0.000000000000000000 ) ) ;
#17367 = DIRECTION ( 'NONE',  ( 0.000000000000000000, 0.000000000000000000, -1.000000000000000000 ) ) ;
#17368 = DIRECTION ( 'NONE',  ( -0.000000000000000000, -0.000000000000000000, 1.000000000000000000 ) ) ;
#17369 = CARTESIAN_POINT ( 'NONE',  ( 9.999999999999998224, 53.26727847779604019, -48.44168704307576689 ) ) ;
#17370 = DIRECTION ( 'NONE',  ( -6.123233995736667428E-17, 1.060575238724912585E-16, -1.000000000000000000 ) ) ;
#17371 = AXIS2_PLACEMENT_3D ( 'NONE', #8856, #5459, #5363 ) ;
#17372 = CARTESIAN_POINT ( 'NONE',  ( -6.888301784570739272, -16.62983158437509701, 7.403862500180310668 ) ) ;
#17373 = EDGE_CURVE ( 'NONE', #13894, #4175, #19338, .T. ) ;
#17374 = CARTESIAN_POINT ( 'NONE',  ( -1.491842754445842800, 7.500000000179346316, -14.86208124981968481 ) ) ;
#17375 = VERTEX_POINT ( 'NONE', #14333 ) ;
#17376 = VECTOR ( 'NONE', #7792, 1000.000000000000000 ) ;
#17377 = PLANE ( 'NONE',  #11098 ) ;
#17378 = AXIS2_PLACEMENT_3D ( 'NONE', #13943, #4394, #20398 ) ;
#17379 = CARTESIAN_POINT ( 'NONE',  ( 12.54593441562639988, -8.382925371439625906, 11.00580183151907754 ) ) ;
#17380 = EDGE_LOOP ( 'NONE', ( #3576, #3260, #10174, #14982 ) ) ;
#17381 = B_SPLINE_CURVE_WITH_KNOTS ( 'NONE', 3,
 ( #6342, #982, #12827, #7425 ),
 .UNSPECIFIED., .F., .F.,
 ( 4, 4 ),
 ( 6.938893903907228378E-18, 0.005429897942433492726 ),
 .UNSPECIFIED. ) ;
#17382 = FACE_OUTER_BOUND ( 'NONE', #13267, .T. ) ;
#17383 = CARTESIAN_POINT ( 'NONE',  ( 0.000000000000000000, 0.000000000000000000, 129.0000000000000000 ) ) ;
#17384 = LINE ( 'NONE', #9010, #938 ) ;
#17385 = CIRCLE ( 'NONE', #20069, 5.000000000000004441 ) ;
#17386 = ORIENTED_EDGE ( 'NONE', *, *, #5731, .T. ) ;
#17387 = EDGE_CURVE ( 'NONE', #1492, #13448, #20780, .T. ) ;
#17388 = DIRECTION ( 'NONE',  ( 1.000000000000000000, 0.000000000000000000, 0.000000000000000000 ) ) ;
#17389 = ORIENTED_EDGE ( 'NONE', *, *, #6746, .T. ) ;
#17390 = CARTESIAN_POINT ( 'NONE',  ( 41.73623995412758347, -13.12544047974070693, -80.94893887662107090 ) ) ;
#17391 = LINE ( 'NONE', #2975, #11078 ) ;
#17392 = ADVANCED_FACE ( 'NONE', ( #12165 ), #19060, .T. ) ;
#17393 = ORIENTED_EDGE ( 'NONE', *, *, #12672, .F. ) ;
#17394 = EDGE_LOOP ( 'NONE', ( #14186, #18815, #17326, #3700 ) ) ;
#17395 = LINE ( 'NONE', #15581, #15459 ) ;
#17396 = AXIS2_PLACEMENT_3D ( 'NONE', #6585, #11569, #13068 ) ;
#17397 = AXIS2_PLACEMENT_3D ( 'NONE', #12534, #7544, #18998 ) ;
#17398 = EDGE_CURVE ( 'NONE', #20061, #11443, #16295, .T. ) ;
#17399 =( NAMED_UNIT ( * ) PLANE_ANGLE_UNIT ( ) SI_UNIT ( $, .RADIAN. ) );
#17400 = DIRECTION ( 'NONE',  ( 1.000000000000000000, 0.000000000000000000, 0.000000000000000000 ) ) ;
#17401 = CARTESIAN_POINT ( 'NONE',  ( 85.00002539999999840, 0.000000000000000000, 4.000000000000000000 ) ) ;
#17402 =( BOUNDED_CURVE ( )  B_SPLINE_CURVE ( 2, ( #2838, #15660, #12590, #1157, #7608, #4534, #10996, #17473, #2950, #15873, #3556, #11208, #20846, #16283, #8332, #177, #16389 ),
 .UNSPECIFIED., .F., .T. ) 
 B_SPLINE_CURVE_WITH_KNOTS ( ( 3, 2, 2, 2, 2, 2, 2, 2, 3 ),
 ( 0.7000000000038510972, 0.7125000000038511638, 0.7250000000038511194, 0.7375000000038511860, 0.7500000000038511416, 0.7625000000038510972, 0.7750000000038511638, 0.7875000000038511194, 0.8000000000038511860 ),
 .UNSPECIFIED. ) 
 CURVE ( )  GEOMETRIC_REPRESENTATION_ITEM ( )  RATIONAL_B_SPLINE_CURVE ( ( 0.9999999999940800688, 0.9807852804091503618, 1.000000000000000000, 0.9807852804032304306, 1.000000000000000000, 0.9807852804032304306, 1.000000000000000000, 0.9807852804032304306, 1.000000000000000000, 0.9807852804032304306, 1.000000000000000000, 0.9807852804032304306, 1.000000000000000000, 0.9807852804032304306, 1.000000000000000000, 0.9807852803973104994, 1.000000000005919931 ) ) 
 REPRESENTATION_ITEM ( '' )  );
#17403 = VECTOR ( 'NONE', #2036, 1000.000000000000000 ) ;
#17404 = AXIS2_PLACEMENT_3D ( 'NONE', #11959, #6971, #13771 ) ;
#17405 = CARTESIAN_POINT ( 'NONE',  ( -11.17563879731704723, 1.343452237168308679E-09, 14.08239024971319964 ) ) ;
#17406 = LINE ( 'NONE', #4361, #728 ) ;
#17407 = ADVANCED_FACE ( 'NONE', ( #2951 ), #9419, .T. ) ;
#17408 = AXIS2_PLACEMENT_3D ( 'NONE', #7875, #20690, #10953 ) ;
#17409 = DIRECTION ( 'NONE',  ( -0.000000000000000000, -0.000000000000000000, -1.000000000000000000 ) ) ;
#17410 = LINE ( 'NONE', #2877, #15764 ) ;
#17411 = ADVANCED_FACE ( 'NONE', ( #7723, #14196, #4536, #4099, #837, #5916 ), #14087, .T. ) ;
#17412 = CIRCLE ( 'NONE', #14697, 7.500000000000000000 ) ;
#17413 = ORIENTED_EDGE ( 'NONE', *, *, #13150, .F. ) ;
#17414 = DIRECTION ( 'NONE',  ( -0.000000000000000000, 1.000000000000000000, 1.224646799147353207E-16 ) ) ;
#17415 = ORIENTED_EDGE ( 'NONE', *, *, #9976, .F. ) ;
#17416 = CARTESIAN_POINT ( 'NONE',  ( 18.00000000000000000, -2.163824016901520184E-09, -16.29604999981969016 ) ) ;
#17417 = CARTESIAN_POINT ( 'NONE',  ( 20.23544477270224817, -7.290198706429656283, 79.18558687180568256 ) ) ;
#17418 = ORIENTED_EDGE ( 'NONE', *, *, #13711, .T. ) ;
#17419 = CARTESIAN_POINT ( 'NONE',  ( 0.000000000000000000, -1.178949249685213863, 2.042000000000002924 ) ) ;
#17420 = VERTEX_POINT ( 'NONE', #950 ) ;
#17421 = FACE_OUTER_BOUND ( 'NONE', #10581, .T. ) ;
#17422 = DIRECTION ( 'NONE',  ( 0.000000000000000000, 0.000000000000000000, -1.000000000000000000 ) ) ;
#17423 = DIRECTION ( 'NONE',  ( 0.000000000000000000, 0.000000000000000000, -1.000000000000000000 ) ) ;
#17424 = ADVANCED_FACE ( 'NONE', ( #9306 ), #18856, .T. ) ;
#17425 = CIRCLE ( 'NONE', #18090, 27.60000000002760245 ) ;
#17426 = ORIENTED_EDGE ( 'NONE', *, *, #5834, .T. ) ;
#17427 = DIRECTION ( 'NONE',  ( -0.000000000000000000, -0.000000000000000000, 1.000000000000000000 ) ) ;
#17428 = CARTESIAN_POINT ( 'NONE',  ( 50.00000000000000000, 31.35083268962912584, 6.892027480330899929E-14 ) ) ;
#17429 = CARTESIAN_POINT ( 'NONE',  ( -18.00000000043040771, -3.580422610670021211, -21.30308124981969442 ) ) ;
#17430 = DIRECTION ( 'NONE',  ( -1.000000000000000000, 0.000000000000000000, -0.000000000000000000 ) ) ;
#17431 = AXIS2_PLACEMENT_3D ( 'NONE', #6680, #13159, #5086 ) ;
#17432 = DIRECTION ( 'NONE',  ( 0.000000000000000000, 0.4999999999999993894, -0.8660254037844389297 ) ) ;
#17433 = ORIENTED_EDGE ( 'NONE', *, *, #6105, .T. ) ;
#17434 = LINE ( 'NONE', #11164, #12380 ) ;
#17435 = CARTESIAN_POINT ( 'NONE',  ( 0.000000000000000000, 51.43306257653197378, -40.15061736769512635 ) ) ;
#17436 = ORIENTED_EDGE ( 'NONE', *, *, #15445, .T. ) ;
#17437 = DIRECTION ( 'NONE',  ( -1.000000000000000000, 0.000000000000000000, -0.000000000000000000 ) ) ;
#17438 = CARTESIAN_POINT ( 'NONE',  ( 50.00000000000000000, -159.9999999999999716, 85.00000000000000000 ) ) ;
#17439 = ORIENTED_EDGE ( 'NONE', *, *, #17774, .F. ) ;
#17440 = CARTESIAN_POINT ( 'NONE',  ( -16.62983158603122291, -6.888301780572501087, -10.26801249981968844 ) ) ;
#17441 = DIRECTION ( 'NONE',  ( -1.000000000000000000, 0.000000000000000000, 0.000000000000000000 ) ) ;
#17442 = CARTESIAN_POINT ( 'NONE',  ( 24.99999999999999645, -122.0000000000000000, -6.368163355566234804E-15 ) ) ;
#17443 = B_SPLINE_CURVE_WITH_KNOTS ( 'NONE', 3,
 ( #2025, #16333, #1634, #14957 ),
 .UNSPECIFIED., .F., .F.,
 ( 4, 4 ),
 ( 2.380737581782212780E-07, 0.002336974151641520864 ),
 .UNSPECIFIED. ) ;
#17444 = ORIENTED_EDGE ( 'NONE', *, *, #1730, .F. ) ;
#17445 = CLOSED_SHELL ( 'NONE', ( #3788, #10515, #4771, #10538, #1967, #7583, #19600, #19029, #12923, #267, #20840, #19520, #15971, #17841, #7149, #30, #2374, #16897, #2369, #20092, #7750, #1024, #15357, #431, #19946, #4942, #16863, #16438, #17593, #3326, #6387, #12687, #2796, #11577, #17799, #9316, #8059, #8459, #10143, #7675, #7562, #2427, #2221, #2878, #956, #5003, #5697, #3028, #8766, #3512, #15905, #247, #11433, #3639, #5726, #925, #3209, #8063, #10362, #16371, #20851, #20359, #15561, #7268, #3765, #9673, #15529, #4528, #16996, #1640, #4556, #9640, #5859, #9978, #5212, #7778, #4836, #1397, #6603, #15032, #7790, #18586, #15251, #11929, #3615, #14653, #6947, #18830, #14042, #18807, #10728, #1955, #14434, #11306, #6128, #5615, #20551, #19148, #20886, #3806, #2729, #20393, #17452, #8308, #7697, #15290, #5719, #16180, #3090, #20148, #5964, #6359, #3759, #3005, #15424, #20356, #11396, #17483, #7163, #12987, #6364, #2106, #1679, #4954, #9089, #13239, #7399, #1072, #16878, #12628, #11827, #18890, #17392, #10384, #12733, #6758, #13014, #15526, #9932, #1039, #17574, #17239, #6348, #18551, #4037, #12177, #5342, #20301, #20089, #7390, #13489, #7473, #1771, #1467, #11066, #1993, #17917, #5876, #14940, #14064, #6631, #18863, #20611, #4543, #2520, #15182, #19280, #13921, #4055, #17145, #1432, #15559, #5995, #4799, #6542, #15432, #5046, #8820, #1458, #9462, #10216, #7145, #19465, #9049, #6918, #917, #1662, #17407, #1231, #3829, #17124, #13508, #1464, #16621, #18736, #8159, #8562, #3287, #3750, #11109, #1552, #3163, #1053 ) ) ;
#17446 = LINE ( 'NONE', #15523, #3462 ) ;
#17447 = ORIENTED_EDGE ( 'NONE', *, *, #16824, .F. ) ;
#17448 = CARTESIAN_POINT ( 'NONE',  ( 2.500000000000000000, 0.000000000000000000, 0.000000000000000000 ) ) ;
#17449 = EDGE_LOOP ( 'NONE', ( #20357, #18771, #19176, #16556 ) ) ;
#17450 = CARTESIAN_POINT ( 'NONE',  ( -11.50000000000000000, 0.000000000000000000, -68.00000000000000000 ) ) ;
#17451 = CARTESIAN_POINT ( 'NONE',  ( 4.000000000000003553, -1.933795701539621659, -5.351162342337697275 ) ) ;
#17452 = ADVANCED_FACE ( 'NONE', ( #13868 ), #7284, .T. ) ;
#17453 = ITEM_DEFINED_TRANSFORMATION ( 'NONE', 'NONE', #15066,  #12461 ) ;
#17454 = CARTESIAN_POINT ( 'NONE',  ( -1.779019326032424922E-09, -14.79893867758297610, -0.7534580811584571380 ) ) ;
#17455 = EDGE_LOOP ( 'NONE', ( #7648, #17218 ) ) ;
#17456 = VECTOR ( 'NONE', #5974, 1000.000000000000000 ) ;
#17457 = CARTESIAN_POINT ( 'NONE',  ( 0.000000000000000000, 0.000000000000000000, 43.00000000000000000 ) ) ;
#17458 = CARTESIAN_POINT ( 'NONE',  ( 2.500000000000000000, 2.357898499370433054, -1.951563910473907981E-15 ) ) ;
#17459 = ORIENTED_EDGE ( 'NONE', *, *, #8425, .T. ) ;
#17460 = CARTESIAN_POINT ( 'NONE',  ( 16.19442412633312856, -14.14534473583932339, 80.24994515060548395 ) ) ;
#17461 = CARTESIAN_POINT ( 'NONE',  ( -1.491842754445841690, 7.500000000179340987, -21.12698124981969272 ) ) ;
#17462 = DIRECTION ( 'NONE',  ( 0.000000000000000000, 0.000000000000000000, 1.000000000000000000 ) ) ;
#17463 = ORIENTED_EDGE ( 'NONE', *, *, #8074, .F. ) ;
#17464 = AXIS2_PLACEMENT_3D ( 'NONE', #10527, #4048, #11614 ) ;
#17465 = FACE_OUTER_BOUND ( 'NONE', #2546, .T. ) ;
#17466 = CARTESIAN_POINT ( 'NONE',  ( 6.250000000000054179, 10.82531754730546147, 43.00000000000000000 ) ) ;
#17467 = ORIENTED_EDGE ( 'NONE', *, *, #9567, .F. ) ;
#17468 = DIRECTION ( 'NONE',  ( 0.000000000000000000, 0.000000000000000000, 1.000000000000000000 ) ) ;
#17469 = AXIS2_PLACEMENT_3D ( 'NONE', #1404, #10932, #12201 ) ;
#17470 = CARTESIAN_POINT ( 'NONE',  ( -4.248408730893246776, -6.358192987158592047, 3.613643750180308256 ) ) ;
#17471 = CARTESIAN_POINT ( 'NONE',  ( -15.25966317163202923, -10.19618095047497874, -21.89214374981969513 ) ) ;
#17472 = ORIENTED_EDGE ( 'NONE', *, *, #15767, .T. ) ;
#17473 = CARTESIAN_POINT ( 'NONE',  ( -1.491842756249033286, -7.499999999820668783, -9.560518749819689077 ) ) ;
#17474 = CARTESIAN_POINT ( 'NONE',  ( 19.99999999999999645, 15.58726123847851142, 62.93731870009410301 ) ) ;
#17475 = EDGE_CURVE ( 'NONE', #14868, #14556, #7609, .T. ) ;
#17476 = CARTESIAN_POINT ( 'NONE',  ( 17.50000000000000355, 2.143131898507868643E-15, 43.00000000000000000 ) ) ;
#17477 = CARTESIAN_POINT ( 'NONE',  ( 7.500000000000001776, -9.015933403756337545E-10, -24.76874999981969694 ) ) ;
#17478 = DIRECTION ( 'NONE',  ( 1.000000000000000000, 0.000000000000000000, 0.000000000000000000 ) ) ;
#17479 = CARTESIAN_POINT ( 'NONE',  ( 2.163825119083639947E-09, 18.00000000000000355, 2.102300000180308714 ) ) ;
#17480 = CARTESIAN_POINT ( 'NONE',  ( 7.500000000000007994, -9.015933403756345817E-10, -12.21129999981968695 ) ) ;
#17481 = ORIENTED_EDGE ( 'NONE', *, *, #11308, .T. ) ;
#17482 = DIRECTION ( 'NONE',  ( -1.000000000000000000, 0.000000000000000000, 0.000000000000000000 ) ) ;
#17483 = ADVANCED_FACE ( 'NONE', ( #20219 ), #4332, .T. ) ;
#17484 = AXIS2_PLACEMENT_3D ( 'NONE', #12352, #4062, #10333 ) ;
#17485 = AXIS2_PLACEMENT_3D ( 'NONE', #19047, #3139, #7802 ) ;
#17486 = CARTESIAN_POINT ( 'NONE',  ( -8.382925368423267187, 12.54593441764186856, 6.882364331519074341 ) ) ;
#17487 = CYLINDRICAL_SURFACE ( 'NONE', #348, 7.500000000000000000 ) ;
#17488 = VERTEX_POINT ( 'NONE', #1047 ) ;
#17489 = CARTESIAN_POINT ( 'NONE',  ( -30.00000000000000000, 40.00000000000000000, -130.0000000000000000 ) ) ;
#17490 = VECTOR ( 'NONE', #544, 1000.000000000000000 ) ;
#17491 = CARTESIAN_POINT ( 'NONE',  ( 18.00000000000000000, -2.163824016901520184E-09, -23.81644999981969235 ) ) ;
#17492 = CARTESIAN_POINT ( 'NONE',  ( -6.177131623262581250, 0.000000000000000000, 0.000000000000000000 ) ) ;
#17493 = ORIENTED_EDGE ( 'NONE', *, *, #11447, .F. ) ;
#17494 = DIRECTION ( 'NONE',  ( -1.000000000000000000, 0.000000000000000000, 0.000000000000000000 ) ) ;
#17495 = CONICAL_SURFACE ( 'NONE', #8338, 2.041999999999999815, 1.047197551196591858 ) ;
#17496 = ORIENTED_EDGE ( 'NONE', *, *, #13129, .T. ) ;
#17497 = CARTESIAN_POINT ( 'NONE',  ( 31.56332346631016961, -35.94799839343871639, -71.81695530636427804 ) ) ;
#17498 = DIRECTION ( 'NONE',  ( 0.000000000000000000, -0.7308359642781300236, 0.6825531432186476843 ) ) ;
#17499 = AXIS2_PLACEMENT_3D ( 'NONE', #719, #13764, #17045 ) ;
#17500 = ORIENTED_EDGE ( 'NONE', *, *, #6369, .T. ) ;
#17501 = ORIENTED_EDGE ( 'NONE', *, *, #16620, .F. ) ;
#17502 = DIRECTION ( 'NONE',  ( -1.000000000000000000, -0.000000000000000000, 0.000000000000000000 ) ) ;
#17503 = VECTOR ( 'NONE', #7887, 1000.000000000000000 ) ;
#17504 = AXIS2_PLACEMENT_3D ( 'NONE', #19765, #16579, #19455 ) ;
#17505 = STYLED_ITEM ( 'NONE', ( #2341 ), #1863 ) ;
#17506 = DIRECTION ( 'NONE',  ( -1.000000000000000000, 0.000000000000000000, 0.000000000000000000 ) ) ;
#17507 = CIRCLE ( 'NONE', #12079, 2.649999999999998579 ) ;
#17508 = DIRECTION ( 'NONE',  ( 0.000000000000000000, -0.5000000000000012212, -0.8660254037844380415 ) ) ;
#17509 = CARTESIAN_POINT ( 'NONE',  ( 2.222972771497741640, 11.17563879704982988, -13.84410899935257788 ) ) ;
#17510 = ADVANCED_FACE ( 'NONE', ( #6115, #15458 ), #7494, .T. ) ;
#17511 = CARTESIAN_POINT ( 'NONE',  ( 1.343451552857795099E-09, 11.17563879731704723, 16.43864024971319893 ) ) ;
#17512 = AXIS2_PLACEMENT_3D ( 'NONE', #15115, #10234, #18510 ) ;
#17513 = EDGE_CURVE ( 'NONE', #18559, #7632, #19676, .T. ) ;
#17514 = DIRECTION ( 'NONE',  ( -0.000000000000000000, -0.000000000000000000, 1.000000000000000000 ) ) ;
#17515 = DIRECTION ( 'NONE',  ( 1.000000000000000000, 0.000000000000000000, 0.000000000000000000 ) ) ;
#17516 = DIRECTION ( 'NONE',  ( -1.000000000000000000, 0.000000000000000000, -0.000000000000000000 ) ) ;
#17517 = VECTOR ( 'NONE', #15446, 1000.000000000000000 ) ;
#17518 = VERTEX_POINT ( 'NONE', #20435 ) ;
#17519 = VECTOR ( 'NONE', #12899, 1000.000000000000000 ) ;
#17520 = CARTESIAN_POINT ( 'NONE',  ( 54.64999999999999858, -39.99999999999999289, 5.000000000000000000 ) ) ;
#17521 = ORIENTED_EDGE ( 'NONE', *, *, #272, .F. ) ;
#17522 = CARTESIAN_POINT ( 'NONE',  ( -12.72792205982779912, 12.72792206288790950, -19.83042499981968732 ) ) ;
#17523 = CARTESIAN_POINT ( 'NONE',  ( 21.25854252069020234, -3.402546668908731586, 82.74447975664143939 ) ) ;
#17524 = ADVANCED_FACE ( 'NONE', ( #10798 ), #17260, .F. ) ;
#17525 = ORIENTED_EDGE ( 'NONE', *, *, #1632, .T. ) ;
#17526 = PRODUCT_DEFINITION ( 'UNKNOWN', '', #16416, #725 ) ;
#17527 = LINE ( 'NONE', #2996, #17743 ) ;
#17528 = ORIENTED_EDGE ( 'NONE', *, *, #2200, .F. ) ;
#17529 = LINE ( 'NONE', #15918, #10181 ) ;
#17530 = CARTESIAN_POINT ( 'NONE',  ( 2.500000000000000000, 2.357898499370433054, -1.951563910473907981E-15 ) ) ;
#17531 = CARTESIAN_POINT ( 'NONE',  ( -30.00000000000000000, -40.00000000000000000, -120.0000000000000142 ) ) ;
#17532 = AXIS2_PLACEMENT_3D ( 'NONE', #7511, #5932, #12403 ) ;
#17533 = ORIENTED_EDGE ( 'NONE', *, *, #1989, .F. ) ;
#17534 = CARTESIAN_POINT ( 'NONE',  ( 19.99999999999999645, 0.000000000000000000, 0.000000000000000000 ) ) ;
#17535 = CARTESIAN_POINT ( 'NONE',  ( 16.62983158437509346, -6.888301784570737496, -25.13198749981969371 ) ) ;
#17536 = CARTESIAN_POINT ( 'NONE',  ( 19.99999999999999645, -20.60847369613026103, 61.90898814327709943 ) ) ;
#17537 = EDGE_CURVE ( 'NONE', #20260, #1747, #9199, .T. ) ;
#17538 = AXIS2_PLACEMENT_3D ( 'NONE', #10944, #14235, #15714 ) ;
#17539 = CARTESIAN_POINT ( 'NONE',  ( 4.248408729364576253, -6.358192988180015881, 11.27145625018030906 ) ) ;
#17540 = ORIENTED_EDGE ( 'NONE', *, *, #20402, .T. ) ;
#17541 = EDGE_CURVE ( 'NONE', #659, #16270, #8189, .T. ) ;
#17542 = CARTESIAN_POINT ( 'NONE',  ( 0.000000000000000000, 0.000000000000000000, 0.000000000000000000 ) ) ;
#17543 = MANIFOLD_SOLID_BREP ( 'Hex', #5831 ) ;
#17544 = EDGE_CURVE ( 'NONE', #11718, #10704, #9625, .T. ) ;
#17545 = CARTESIAN_POINT ( 'NONE',  ( -9.015947181032835626E-10, -7.500000000000007994, -0.4300499998196871676 ) ) ;
#17547 = ORIENTED_EDGE ( 'NONE', *, *, #16424, .F. ) ;
#17546 = APPLICATION_CONTEXT ( 'automotive_design' ) ;
#17548 = LINE ( 'NONE', #14364, #4398 ) ;
#17549 = LINE ( 'NONE', #9474, #797 ) ;
#17550 = EDGE_CURVE ( 'NONE', #4504, #14189, #19031, .T. ) ;
#17551 = ORIENTED_EDGE ( 'NONE', *, *, #9379, .T. ) ;
#17552 = AXIS2_PLACEMENT_3D ( 'NONE', #8817, #18168, #18265 ) ;
#17553 = CARTESIAN_POINT ( 'NONE',  ( -15.25966317163203279, -10.19618095047498052, -10.56254374981968880 ) ) ;
#17554 = CARTESIAN_POINT ( 'NONE',  ( -11.49999999999998934, -85.00000000000000000, 19.00000000000000000 ) ) ;
#17555 = CARTESIAN_POINT ( 'NONE',  ( 19.99999999999999645, 58.26603306961962403, 42.29739224042491941 ) ) ;
#17556 = EDGE_LOOP ( 'NONE', ( #8814, #20147, #20802, #19988 ) ) ;
#17557 = CARTESIAN_POINT ( 'NONE',  ( -9.850000000000019185, 0.000000000000000000, 46.00000000000000711 ) ) ;
#17558 = ORIENTED_EDGE ( 'NONE', *, *, #20171, .T. ) ;
#17559 = CARTESIAN_POINT ( 'NONE',  ( 50.00000000000000000, -151.4095880458873467, -44.60680010464253087 ) ) ;
#17560 = ORIENTED_EDGE ( 'NONE', *, *, #17653, .T. ) ;
#17561 = CARTESIAN_POINT ( 'NONE',  ( 0.000000000000000000, 0.000000000000000000, 0.000000000000000000 ) ) ;
#17562 = EDGE_CURVE ( 'NONE', #5841, #20820, #9513, .T. ) ;
#17563 = CARTESIAN_POINT ( 'NONE',  ( 0.000000000000000000, 0.000000000000000000, 40.00000000000000000 ) ) ;
#17564 = CARTESIAN_POINT ( 'NONE',  ( 2.943691925285398803, -14.79893867793684059, -19.89798933115845969 ) ) ;
#17565 = ORIENTED_EDGE ( 'NONE', *, *, #8702, .T. ) ;
#17566 = CARTESIAN_POINT ( 'NONE',  ( 7.500000000000000000, -1.491842755816076060, -18.18166874991221249 ) ) ;
#17567 = CARTESIAN_POINT ( 'NONE',  ( 0.000000000000000000, 60.40676135667438729, 23.56039007469059143 ) ) ;
#17568 = ORIENTED_EDGE ( 'NONE', *, *, #15265, .T. ) ;
#17569 = DIRECTION ( 'NONE',  ( 0.000000000000000000, 0.000000000000000000, -1.000000000000000000 ) ) ;
#17570 = CARTESIAN_POINT ( 'NONE',  ( 6.358192988180014993, 4.248408729364578917, -19.35979374981969769 ) ) ;
#17571 = FACE_OUTER_BOUND ( 'NONE', #7089, .T. ) ;
#17572 = ORIENTED_EDGE ( 'NONE', *, *, #10127, .F. ) ;
#17573 = MANIFOLD_SOLID_BREP ( 'Mirror1', #18366 ) ;
#17574 = ADVANCED_FACE ( 'NONE', ( #14404 ), #12818, .T. ) ;
#17575 = CARTESIAN_POINT ( 'NONE',  ( -2.339468227445729021, -3.268109542640674547, -1.786138375875142494E-14 ) ) ;
#17576 = CARTESIAN_POINT ( 'NONE',  ( 10.00000000000000178, -164.9999999999999716, -73.20000000000000284 ) ) ;
#17577 = ORIENTED_EDGE ( 'NONE', *, *, #16034, .F. ) ;
#17578 = DIRECTION ( 'NONE',  ( -1.551631016079434660E-16, 1.000000000000000000, 0.000000000000000000 ) ) ;
#17579 = LINE ( 'NONE', #19258, #10342 ) ;
#17580 = FACE_OUTER_BOUND ( 'NONE', #16879, .T. ) ;
#17581 = EDGE_LOOP ( 'NONE', ( #11231, #9775, #16916, #69 ) ) ;
#17582 = DIRECTION ( 'NONE',  ( 0.000000000000000000, -0.000000000000000000, -1.000000000000000000 ) ) ;
#17583 = SURFACE_STYLE_FILL_AREA ( #1579 ) ;
#17584 = DIRECTION ( 'NONE',  ( 0.000000000000000000, 0.000000000000000000, 1.000000000000000000 ) ) ;
#17585 = DIRECTION ( 'NONE',  ( -0.9237280213470682178, -0.3830490080632377725, 1.243481486083095525E-31 ) ) ;
#17586 = CARTESIAN_POINT ( 'NONE',  ( -3.580422610670018990, 18.00000000043041481, -17.04223124981969306 ) ) ;
#17587 = CARTESIAN_POINT ( 'NONE',  ( 52.00000000000000000, -99.99999999999998579, 5.000000000000000000 ) ) ;
#17588 = ORIENTED_EDGE ( 'NONE', *, *, #6976, .F. ) ;
#17589 = DIRECTION ( 'NONE',  ( 0.000000000000000000, 0.6310879443260485333, 0.7757112907044232397 ) ) ;
#17590 = CARTESIAN_POINT ( 'NONE',  ( 10.46442989454075168, 10.46442989202483886, 18.36908308151907576 ) ) ;
#17591 = DIRECTION ( 'NONE',  ( -1.836909530733573776E-16, 1.000000000000000000, 0.000000000000000000 ) ) ;
#17592 = ORIENTED_EDGE ( 'NONE', *, *, #7421, .T. ) ;
#17593 = ADVANCED_FACE ( 'NONE', ( #475 ), #18169, .T. ) ;
#17594 = DIRECTION ( 'NONE',  ( -0.000000000000000000, 0.000000000000000000, 1.000000000000000000 ) ) ;
#17595 = FACE_OUTER_BOUND ( 'NONE', #13796, .T. ) ;
#17596 = DIRECTION ( 'NONE',  ( 0.000000000000000000, 0.000000000000000000, 1.000000000000000000 ) ) ;
#17597 = ORIENTED_EDGE ( 'NONE', *, *, #9374, .F. ) ;
#17598 = CARTESIAN_POINT ( 'NONE',  ( 19.99999999999999645, 0.000000000000000000, 0.000000000000000000 ) ) ;
#17599 = ORIENTED_EDGE ( 'NONE', *, *, #15807, .T. ) ;
#17600 = CARTESIAN_POINT ( 'NONE',  ( 19.99999999999999645, 24.01204443665187327, 60.22865198596132785 ) ) ;
#17601 = CARTESIAN_POINT ( 'NONE',  ( 62.49999999999999289, -40.00000000000000000, 0.000000000000000000 ) ) ;
#17602 = ORIENTED_EDGE ( 'NONE', *, *, #17513, .F. ) ;
#17603 = ORIENTED_EDGE ( 'NONE', *, *, #13394, .F. ) ;
#17604 = CARTESIAN_POINT ( 'NONE',  ( 19.99999999999999645, 27.62776854598856602, 58.65812137499012380 ) ) ;
#17605 = AXIS2_PLACEMENT_3D ( 'NONE', #4932, #367, #8516 ) ;
#17606 = CYLINDRICAL_SURFACE ( 'NONE', #16690, 27.60000000002759535 ) ;
#17607 = DIRECTION ( 'NONE',  ( 0.000000000000000000, 0.000000000000000000, -1.000000000000000000 ) ) ;
#17608 = CARTESIAN_POINT ( 'NONE',  ( 4.276731812588570492, -10.32494394809439697, -10.01520274935256971 ) ) ;
#17609 = CARTESIAN_POINT ( 'NONE',  ( -11.17563879704981922, 2.222972771497742972, 14.37692149971319999 ) ) ;
#17610 = LINE ( 'NONE', #15804, #2422 ) ;
#17611 = DIRECTION ( 'NONE',  ( -1.000000000000000000, 0.000000000000000000, -0.000000000000000000 ) ) ;
#17612 = CARTESIAN_POINT ( 'NONE',  ( 19.99999999999999645, 28.84646472442454979, 58.52617768068444093 ) ) ;
#17613 = ORIENTED_EDGE ( 'NONE', *, *, #5186, .F. ) ;
#17614 = CARTESIAN_POINT ( 'NONE',  ( 6.250000000000054179, 10.82531754730546147, 126.0000000000000000 ) ) ;
#17615 = VERTEX_POINT ( 'NONE', #5234 ) ;
#17616 = CARTESIAN_POINT ( 'NONE',  ( -18.00000000043041126, -3.580422610670022543, -21.30308124981969087 ) ) ;
#17617 = LINE ( 'NONE', #9039, #836 ) ;
#17618 = ORIENTED_EDGE ( 'NONE', *, *, #6690, .T. ) ;
#17619 = DIRECTION ( 'NONE',  ( -0.000000000000000000, -0.000000000000000000, 1.000000000000000000 ) ) ;
#17620 = VERTEX_POINT ( 'NONE', #3638 ) ;
#17621 = DIRECTION ( 'NONE',  ( -0.000000000000000000, -0.000000000000000000, -1.000000000000000000 ) ) ;
#17622 = DIRECTION ( 'NONE',  ( 0.000000000000000000, 0.000000000000000000, 1.000000000000000000 ) ) ;
#17623 = FACE_OUTER_BOUND ( 'NONE', #20477, .T. ) ;
#17624 = ORIENTED_EDGE ( 'NONE', *, *, #11168, .T. ) ;
#17625 = CARTESIAN_POINT ( 'NONE',  ( 19.99999999999999645, 0.000000000000000000, 0.000000000000000000 ) ) ;
#17626 = EDGE_CURVE ( 'NONE', #18991, #14005, #16312, .T. ) ;
#17627 = EDGE_CURVE ( 'NONE', #14303, #12727, #4803, .T. ) ;
#17628 = DIRECTION ( 'NONE',  ( -0.000000000000000000, -0.000000000000000000, 1.000000000000000000 ) ) ;
#17629 = DIRECTION ( 'NONE',  ( 0.000000000000000000, 0.000000000000000000, 1.000000000000000000 ) ) ;
#17630 = CIRCLE ( 'NONE', #12, 10.79377999999999993 ) ;
#17631 = CARTESIAN_POINT ( 'NONE',  ( -44.00000000000000000, -85.00000000000000000, -11.50000000000000711 ) ) ;
#17632 = EDGE_CURVE ( 'NONE', #9751, #5132, #7162, .T. ) ;
#17633 = EDGE_CURVE ( 'NONE', #9351, #12808, #5807, .T. ) ;
#17634 = VERTEX_POINT ( 'NONE', #8755 ) ;
#17635 = CARTESIAN_POINT ( 'NONE',  ( 50.00000000000000000, -159.9999999999999716, -85.00000000000000000 ) ) ;
#17636 = AXIS2_PLACEMENT_3D ( 'NONE', #13584, #5411, #11995 ) ;
#17637 = CARTESIAN_POINT ( 'NONE',  ( -24.99999999999999289, -85.00000000000000000, -1.040949779275250179E-14 ) ) ;
#17638 = AXIS2_PLACEMENT_3D ( 'NONE', #4267, #7656, #17208 ) ;
#17639 = ORIENTED_EDGE ( 'NONE', *, *, #7889, .F. ) ;
#17640 = LINE ( 'NONE', #1333, #5884 ) ;
#17641 = DIRECTION ( 'NONE',  ( 0.000000000000000000, 0.000000000000000000, -1.000000000000000000 ) ) ;
#17642 = VERTEX_POINT ( 'NONE', #18837 ) ;
#17643 = CARTESIAN_POINT ( 'NONE',  ( 30.00000000000000000, -122.0000000000000000, -6.368163355566234804E-15 ) ) ;
#17644 = DIRECTION ( 'NONE',  ( 0.000000000000000000, 8.881784197001252323E-16, 1.000000000000000000 ) ) ;
#17645 = CARTESIAN_POINT ( 'NONE',  ( 0.000000000000000000, -38.69327817041812523, 52.53819777490620169 ) ) ;
#17646 = ORIENTED_EDGE ( 'NONE', *, *, #12715, .F. ) ;
#17647 = EDGE_CURVE ( 'NONE', #5928, #17279, #1096, .T. ) ;
#17648 = CARTESIAN_POINT ( 'NONE',  ( 11.50000000000000000, 1.408343819019456176E-15, -81.99999999999998579 ) ) ;
#17649 = ORIENTED_EDGE ( 'NONE', *, *, #10784, .F. ) ;
#17650 = FACE_OUTER_BOUND ( 'NONE', #17024, .T. ) ;
#17651 = ORIENTED_EDGE ( 'NONE', *, *, #16344, .F. ) ;
#17652 = EDGE_CURVE ( 'NONE', #18871, #833, #4202, .T. ) ;
#17653 = EDGE_CURVE ( 'NONE', #8626, #10526, #13535, .T. ) ;
#17654 = CIRCLE ( 'NONE', #13243, 27.60000000002759890 ) ;
#17655 = CARTESIAN_POINT ( 'NONE',  ( 30.00000000000000000, -85.00000000000000000, -1.040949779275250179E-14 ) ) ;
#17656 = ADVANCED_FACE ( 'NONE', ( #8647 ), #10352, .T. ) ;
#17657 = DIRECTION ( 'NONE',  ( 0.000000000000000000, 0.000000000000000000, -1.000000000000000000 ) ) ;
#17658 = AXIS2_PLACEMENT_3D ( 'NONE', #11140, #19289, #6 ) ;
#17659 = CARTESIAN_POINT ( 'NONE',  ( 1.779017513685136568E-09, 14.79893867758297610, -14.89095808115845720 ) ) ;
#17660 = ORIENTED_EDGE ( 'NONE', *, *, #15088, .F. ) ;
#17661 = CARTESIAN_POINT ( 'NONE',  ( 19.99999999999999645, -15.58726123847893774, 62.93731870009398932 ) ) ;
#17662 = CARTESIAN_POINT ( 'NONE',  ( 2.500000000000000000, -1.178949249685214307, 2.042000000000001592 ) ) ;
#17663 = VERTEX_POINT ( 'NONE', #17138 ) ;
#17664 = VECTOR ( 'NONE', #6766, 1000.000000000000000 ) ;
#17665 = LINE ( 'NONE', #11193, #19284 ) ;
#17666 = CARTESIAN_POINT ( 'NONE',  ( -15.25966316918061771, 10.19618095414378622, 19.47964375018031546 ) ) ;
#17667 = CIRCLE ( 'NONE', #11553, 65.24900000006525147 ) ;
#17668 = FACE_BOUND ( 'NONE', #6759, .T. ) ;
#17669 = LINE ( 'NONE', #15864, #209 ) ;
#17670 = EDGE_CURVE ( 'NONE', #12259, #6658, #4034, .T. ) ;
#17671 = EDGE_CURVE ( 'NONE', #20728, #2251, #1029, .T. ) ;
#17672 = EDGE_LOOP ( 'NONE', ( #139, #19621, #947, #12861 ) ) ;
#17673 = DIRECTION ( 'NONE',  ( -0.000000000000000000, 0.000000000000000000, 1.000000000000000000 ) ) ;
#17674 = CARTESIAN_POINT ( 'NONE',  ( 24.99999999999999645, -122.0000000000000000, -2.100000000000004086 ) ) ;
#17675 = AXIS2_PLACEMENT_3D ( 'NONE', #2303, #15125, #928 ) ;
#17676 = ORIENTED_EDGE ( 'NONE', *, *, #15296, .F. ) ;
#17677 = DIRECTION ( 'NONE',  ( 1.000000000000000000, 0.000000000000000000, 0.000000000000000000 ) ) ;
#17678 = CARTESIAN_POINT ( 'NONE',  ( 0.000000000000000000, 0.000000000000000000, 0.000000000000000000 ) ) ;
#17679 = CYLINDRICAL_SURFACE ( 'NONE', #8910, 17.50000000000000355 ) ;
#17680 = EDGE_CURVE ( 'NONE', #11011, #10195, #3874, .T. ) ;
#17681 = VERTEX_POINT ( 'NONE', #7056 ) ;
#17682 = FACE_BOUND ( 'NONE', #2594, .T. ) ;
#17683 = AXIS2_PLACEMENT_3D ( 'NONE', #5917, #2953, #18858 ) ;
#17684 = CARTESIAN_POINT ( 'NONE',  ( 50.00000000000000000, 36.35083268962920044, -90.00000000000000000 ) ) ;
#17685 = CARTESIAN_POINT ( 'NONE',  ( 19.99999999999999645, 44.69367065308721720, -56.44887778834701919 ) ) ;
#17686 = AXIS2_PLACEMENT_3D ( 'NONE', #16858, #2228, #11664 ) ;
#17687 = CARTESIAN_POINT ( 'NONE',  ( 0.000000000000000000, 0.000000000000000000, 0.000000000000000000 ) ) ;
#17688 = CARTESIAN_POINT ( 'NONE',  ( 2.163825119083639947E-09, 18.00000000000000355, -7.322699999819691108 ) ) ;
#17689 = CARTESIAN_POINT ( 'NONE',  ( 30.00000000000000000, -39.99999999999999289, -52.00000000000000000 ) ) ;
#17690 = LINE ( 'NONE', #3161, #4314 ) ;
#17691 = CARTESIAN_POINT ( 'NONE',  ( -8.382925371439625906, -12.54593441562639988, -5.487948168480926370 ) ) ;
#17692 = DIRECTION ( 'NONE',  ( -1.000000000000000000, -0.000000000000000000, -0.000000000000000000 ) ) ;
#17693 = CIRCLE ( 'NONE', #8528, 27.60000000002760601 ) ;
#17694 = CIRCLE ( 'NONE', #20026, 72.00000000007199219 ) ;
#17695 = ORIENTED_EDGE ( 'NONE', *, *, #18827, .F. ) ;
#17696 = CLOSED_SHELL ( 'NONE', ( #15437, #3, #2901, #18280, #11181, #17524, #3024, #12876, #11077, #818, #19091, #1038, #1978, #3506, #86, #7450, #5447, #19292, #15676, #3520, #8913, #55, #6047, #11911, #12712, #12364, #3429, #6906, #17411, #4845, #7788, #16727, #16596, #10006, #7935, #11806, #3597, #14185, #4566, #12519, #18961, #15076, #895, #4904, #3233, #8304, #19865, #13750, #9753, #1599, #18919, #20470, #2708, #5929, #11687, #19357, #9577, #5317, #17656, #15571, #12670, #10504, #10088, #15506, #4574, #12621, #17802, #3380, #14682, #4301, #5, #20495, #15471, #6691, #20463, #5045, #16362, #20809, #18407, #17241, #19451, #534, #20063, #5254, #8169, #8816, #20927, #3262, #12739, #19596, #2504, #10295, #12986, #6311, #8971, #9918, #236, #5570, #11710, #19456, #2066, #8445, #10453, #13336, #2479, #13529, #10148, #436, #3270, #11779, #14219, #7825, #18642, #9628, #20329, #922, #6511, #13978, #17273, #11055, #732, #18032, #14628, #17093, #12865, #7243, #2627, #13190, #16756 ) ) ;
#17697 = CARTESIAN_POINT ( 'NONE',  ( 1.040949779275250179E-14, -85.00000000000000000, 0.000000000000000000 ) ) ;
#17698 = CARTESIAN_POINT ( 'NONE',  ( 1.491842756249030399, 7.499999999820669672, 23.42698125018031519 ) ) ;
#17699 = CARTESIAN_POINT ( 'NONE',  ( 9.999999999999998224, 53.26727847779537228, 48.44168704307649875 ) ) ;
#17700 = CIRCLE ( 'NONE', #7527, 2.099999999999997868 ) ;
#17701 = EDGE_LOOP ( 'NONE', ( #6411, #9304, #13236, #11669 ) ) ;
#17702 = FACE_OUTER_BOUND ( 'NONE', #12018, .T. ) ;
#17703 = ORIENTED_EDGE ( 'NONE', *, *, #2089, .F. ) ;
#17704 = CARTESIAN_POINT ( 'NONE',  ( 10.00000000000000178, -164.9999999999999716, -70.00000000000000000 ) ) ;
#17705 = CARTESIAN_POINT ( 'NONE',  ( -24.99999999999999289, -30.00000000000000711, -50.99019513592786268 ) ) ;
#17706 = ORIENTED_EDGE ( 'NONE', *, *, #19965, .T. ) ;
#17707 = AXIS2_PLACEMENT_3D ( 'NONE', #1353, #1027, #18725 ) ;
#17708 = ORIENTED_EDGE ( 'NONE', *, *, #1907, .F. ) ;
#17709 = DIRECTION ( 'NONE',  ( -0.000000000000000000, 1.000000000000000000, 1.224646799147353207E-16 ) ) ;
#17710 = DIRECTION ( 'NONE',  ( 0.000000000000000000, -0.9422609221188237294, 0.3348796121709771700 ) ) ;
#17711 = AXIS2_PLACEMENT_3D ( 'NONE', #14906, #19664, #18292 ) ;
#17712 = VECTOR ( 'NONE', #4609, 1000.000000000000000 ) ;
#17713 = EDGE_CURVE ( 'NONE', #1684, #6196, #18962, .T. ) ;
#17714 = PRESENTATION_STYLE_ASSIGNMENT (( #8368 ) ) ;
#17716 = AXIS2_PLACEMENT_3D ( 'NONE', #2388, #10553, #10341 ) ;
#17715 = CARTESIAN_POINT ( 'NONE',  ( 5.303300859536635770, 5.303300858261589923, 24.31057500018031803 ) ) ;
#17717 = CARTESIAN_POINT ( 'NONE',  ( 6.330490856366289165, -9.474249098604506258, 1.417546499713196795 ) ) ;
#17718 = DIRECTION ( 'NONE',  ( -1.000000000000000000, 0.000000000000000000, 0.000000000000000000 ) ) ;
#17719 = CARTESIAN_POINT ( 'NONE',  ( 30.00000000000000000, -85.00000000000000000, 74.99999999999998579 ) ) ;
#17720 = DIRECTION ( 'NONE',  ( 0.000000000000000000, -0.9976687691905384847, -0.06824241336468166164 ) ) ;
#17721 = CIRCLE ( 'NONE', #9261, 16.99999999999995381 ) ;
#17722 = EDGE_LOOP ( 'NONE', ( #2939, #8591, #402, #19245 ) ) ;
#17723 = DIRECTION ( 'NONE',  ( 0.000000000000000000, 1.000000000000000000, -1.471414886128461471E-15 ) ) ;
#17724 = EDGE_LOOP ( 'NONE', ( #18764, #16187, #8412, #397, #11549, #19057 ) ) ;
#17725 = CARTESIAN_POINT ( 'NONE',  ( -12.72792205982779912, 12.72792206288790950, 19.77417500018031404 ) ) ;
#17726 = LINE ( 'NONE', #1522, #14043 ) ;
#17727 = CIRCLE ( 'NONE', #14679, 2.649999999999993694 ) ;
#17728 = VERTEX_POINT ( 'NONE', #8859 ) ;
#17729 = AXIS2_PLACEMENT_3D ( 'NONE', #570, #7020, #11794 ) ;
#17730 = LINE ( 'NONE', #17933, #20440 ) ;
#17731 = VERTEX_POINT ( 'NONE', #13746 ) ;
#17732 = CARTESIAN_POINT ( 'NONE',  ( 50.00000000000000000, 230.0000000000000000, 0.000000000000000000 ) ) ;
#17733 = CARTESIAN_POINT ( 'NONE',  ( 30.00000000000000000, -50.00000000000000000, 71.93747284969079203 ) ) ;
#17734 = ORIENTED_EDGE ( 'NONE', *, *, #10637, .T. ) ;
#17735 = ORIENTED_EDGE ( 'NONE', *, *, #19234, .F. ) ;
#17736 = CARTESIAN_POINT ( 'NONE',  ( 19.99999999999999645, -43.56693332842751687, -48.57318520917550586 ) ) ;
#17737 = DIRECTION ( 'NONE',  ( -1.000000000000000000, 0.000000000000000000, -0.000000000000000000 ) ) ;
#17738 = CARTESIAN_POINT ( 'NONE',  ( 4.000000000000003553, 1.935983797701078757, -0.2494693066162350648 ) ) ;
#17739 = AXIS2_PLACEMENT_3D ( 'NONE', #10376, #4104, #11852 ) ;
#17740 = EDGE_CURVE ( 'NONE', #764, #18535, #19951, .T. ) ;
#17741 = DIRECTION ( 'NONE',  ( 1.000000000000000000, 0.000000000000000000, 0.000000000000000000 ) ) ;
#17742 = AXIS2_PLACEMENT_3D ( 'NONE', #9466, #12663, #14244 ) ;
#17744 = EDGE_LOOP ( 'NONE', ( #19107, #17649, #20673, #1691, #11886 ) ) ;
#17743 = VECTOR ( 'NONE', #20478, 1000.000000000000000 ) ;
#17745 = VECTOR ( 'NONE', #4607, 1000.000000000000000 ) ;
#17746 = CARTESIAN_POINT ( 'NONE',  ( 3.599999999999902833, -10.82531754730554496, 43.00000000000000000 ) ) ;
#17747 = CARTESIAN_POINT ( 'NONE',  ( -9.850000000000019185, 3.245314017740474129E-16, 126.0000000000000000 ) ) ;
#17748 = DIRECTION ( 'NONE',  ( 0.000000000000000000, -0.1361666490962538945, 0.9906859460363297565 ) ) ;
#17749 = DIRECTION ( 'NONE',  ( -1.000000000000000000, 0.000000000000000000, -0.000000000000000000 ) ) ;
#17750 = EDGE_CURVE ( 'NONE', #10368, #12982, #19020, .T. ) ;
#17751 = VERTEX_POINT ( 'NONE', #18939 ) ;
#17752 = CARTESIAN_POINT ( 'NONE',  ( 19.99999999999999645, 0.000000000000000000, 0.000000000000000000 ) ) ;
#17753 = DIRECTION ( 'NONE',  ( -1.000000000000000000, 0.000000000000000000, 0.000000000000000000 ) ) ;
#17754 = CARTESIAN_POINT ( 'NONE',  ( 8.899999999999895550, -10.82531754730554496, 43.00000000000000000 ) ) ;
#17755 = CIRCLE ( 'NONE', #827, 27.60000000002759890 ) ;
#17756 = ORIENTED_EDGE ( 'NONE', *, *, #18042, .T. ) ;
#17757 = DIRECTION ( 'NONE',  ( -1.597351267013635284E-16, 1.000000000000000000, 0.000000000000000000 ) ) ;
#17758 = VERTEX_POINT ( 'NONE', #20522 ) ;
#17759 = DIRECTION ( 'NONE',  ( 0.000000000000000000, 0.000000000000000000, 1.000000000000000000 ) ) ;
#17760 = EDGE_LOOP ( 'NONE', ( #14996, #8197, #11281, #20276, #5111 ) ) ;
#17761 = CIRCLE ( 'NONE', #8597, 27.60000000002760245 ) ;
#17762 = EDGE_CURVE ( 'NONE', #7264, #14245, #15557, .T. ) ;
#17763 = VECTOR ( 'NONE', #1716, 1000.000000000000000 ) ;
#17764 = DIRECTION ( 'NONE',  ( -1.000000000000000000, 0.000000000000000000, 0.000000000000000000 ) ) ;
#17765 = DIRECTION ( 'NONE',  ( 0.000000000000000000, 1.000000000000000000, 0.000000000000000000 ) ) ;
#17766 = CARTESIAN_POINT ( 'NONE',  ( 7.902369978624329327, 7.902369976724401113, 24.73948475064743135 ) ) ;
#17767 = ORIENTED_EDGE ( 'NONE', *, *, #10600, .F. ) ;
#17768 = DIRECTION ( 'NONE',  ( 1.000000000000000000, -0.000000000000000000, 0.000000000000000000 ) ) ;
#17769 = FACE_OUTER_BOUND ( 'NONE', #11584, .T. ) ;
#17770 = VERTEX_POINT ( 'NONE', #10875 ) ;
#17771 = CARTESIAN_POINT ( 'NONE',  ( -10.00000000000000000, 0.000000000000000000, 0.000000000000000000 ) ) ;
#17772 = EDGE_CURVE ( 'NONE', #11773, #4597, #1703, .T. ) ;
#17773 = AXIS2_PLACEMENT_3D ( 'NONE', #16570, #19554, #11493 ) ;
#17774 = EDGE_CURVE ( 'NONE', #17728, #12535, #12804, .T. ) ;
#17775 = DIRECTION ( 'NONE',  ( 0.000000000000000000, 0.000000000000000000, 1.000000000000000000 ) ) ;
#17776 = CYLINDRICAL_SURFACE ( 'NONE', #14485, 21.50000000000000000 ) ;
#17777 = DIRECTION ( 'NONE',  ( -1.000000000000000000, -0.000000000000000000, -0.000000000000000000 ) ) ;
#17778 = ORIENTED_EDGE ( 'NONE', *, *, #12180, .T. ) ;
#17779 = EDGE_CURVE ( 'NONE', #11144, #14849, #17665, .T. ) ;
#17780 = CARTESIAN_POINT ( 'NONE',  ( -4.000000000000000000, -2.309401076758531346, -0.3572655899081733644 ) ) ;
#17781 = EDGE_CURVE ( 'NONE', #7039, #7171, #20287, .T. ) ;
#17782 = ORIENTED_EDGE ( 'NONE', *, *, #18256, .T. ) ;
#17783 = PRODUCT_DEFINITION ( 'UNKNOWN', '', #6270, #13665 ) ;
#17784 = FACE_OUTER_BOUND ( 'NONE', #20620, .T. ) ;
#17785 = CARTESIAN_POINT ( 'NONE',  ( 0.000000000000000000, 31.17893654894229982, 57.31758819669181548 ) ) ;
#17786 = DIRECTION ( 'NONE',  ( 1.000000000000000000, 1.836909530733573776E-16, 0.000000000000000000 ) ) ;
#17787 = EDGE_LOOP ( 'NONE', ( #10765, #11171, #8052, #3677 ) ) ;
#17788 = LINE ( 'NONE', #3254, #18873 ) ;
#17789 = AXIS2_PLACEMENT_3D ( 'NONE', #12994, #9800, #2169 ) ;
#17790 = CARTESIAN_POINT ( 'NONE',  ( -31.75000000000000000, 0.000000000000000000, 0.000000000000000000 ) ) ;
#17791 = DIRECTION ( 'NONE',  ( 6.123233995736814107E-17, 1.060575238724903957E-16, -1.000000000000000000 ) ) ;
#17792 = CARTESIAN_POINT ( 'NONE',  ( 17.99999999956958519, -3.580422614997676778, -4.671918749819693240 ) ) ;
#17793 = EDGE_CURVE ( 'NONE', #2751, #20518, #10889, .T. ) ;
#17794 = ORIENTED_EDGE ( 'NONE', *, *, #13625, .T. ) ;
#17795 = CARTESIAN_POINT ( 'NONE',  ( 30.00000000000000000, -85.00000000000000000, -1.040949779275250179E-14 ) ) ;
#17796 = DIRECTION ( 'NONE',  ( -1.000000000000000000, -0.000000000000000000, 0.000000000000000000 ) ) ;
#17797 = CARTESIAN_POINT ( 'NONE',  ( -12.54593441764187034, -8.382925368423267187, -14.32388566848092992 ) ) ;
#17798 = CIRCLE ( 'NONE', #4257, 11.50000000000000000 ) ;
#17799 = ADVANCED_FACE ( 'NONE', ( #486 ), #12997, .T. ) ;
#17800 = DIRECTION ( 'NONE',  ( -1.000000000000000000, 0.000000000000000000, 0.000000000000000000 ) ) ;
#17801 = CIRCLE ( 'NONE', #6945, 27.60000000002760245 ) ;
#17802 = ADVANCED_FACE ( 'NONE', ( #13100 ), #18182, .F. ) ;
#17803 = VERTEX_POINT ( 'NONE', #8316 ) ;
#17804 = CARTESIAN_POINT ( 'NONE',  ( 0.000000000000000000, 63.17103598352149874, -16.33561182745074447 ) ) ;
#17805 = CARTESIAN_POINT ( 'NONE',  ( 0.000000000000000000, -2.357898499370432610, 3.252606517456513302E-15 ) ) ;
#17806 = FACE_OUTER_BOUND ( 'NONE', #14452, .T. ) ;
#17807 = ORIENTED_EDGE ( 'NONE', *, *, #17626, .F. ) ;
#17808 = CYLINDRICAL_SURFACE ( 'NONE', #8534, 72.00000000007199219 ) ;
#17809 = ORIENTED_EDGE ( 'NONE', *, *, #20751, .T. ) ;
#17810 = DIRECTION ( 'NONE',  ( -1.000000000000000000, -0.000000000000000000, -0.000000000000000000 ) ) ;
#17811 = CARTESIAN_POINT ( 'NONE',  ( -17.99999999999999645, 2.163826221265758470E-09, 16.69145000018031055 ) ) ;
#17812 = ORIENTED_EDGE ( 'NONE', *, *, #12398, .F. ) ;
#17813 = EDGE_LOOP ( 'NONE', ( #20471, #18393 ) ) ;
#17814 = DIRECTION ( 'NONE',  ( -1.000000000000000000, -0.000000000000000000, -0.000000000000000000 ) ) ;
#17815 = CIRCLE ( 'NONE', #16117, 2.041999999999999815 ) ;
#17816 = CARTESIAN_POINT ( 'NONE',  ( 6.250000000000054179, 10.82531754730546147, 40.00000000000000000 ) ) ;
#17817 =( REPRESENTATION_RELATIONSHIP ('NONE','NONE', #13739, #2344 ) REPRESENTATION_RELATIONSHIP_WITH_TRANSFORMATION ( #2926 )SHAPE_REPRESENTATION_RELATIONSHIP( ) );
#17818 = SURFACE_STYLE_FILL_AREA ( #14534 ) ;
#17819 = CARTESIAN_POINT ( 'NONE',  ( 2.500000000000000000, 2.357898499370431722, -2.818925648462311528E-15 ) ) ;
#17820 = ADVANCED_FACE ( 'NONE', ( #5130 ), #5345, .F. ) ;
#17821 = CIRCLE ( 'NONE', #18472, 11.50000000000000000 ) ;
#17822 = FACE_OUTER_BOUND ( 'NONE', #5113, .T. ) ;
#17823 = CARTESIAN_POINT ( 'NONE',  ( 9.015937996181842420E-10, 7.500000000000007994, 13.70745000018031590 ) ) ;
#17824 = CARTESIAN_POINT ( 'NONE',  ( 11.17563879704981566, -2.222972771497744304, 0.2394214997131979827 ) ) ;
#17825 = AXIS2_PLACEMENT_3D ( 'NONE', #2156, #18475, #8930 ) ;
#17826 = DIRECTION ( 'NONE',  ( -0.000000000000000000, -0.000000000000000000, -1.000000000000000000 ) ) ;
#17827 = LINE ( 'NONE', #17719, #13179 ) ;
#17828 = DIRECTION ( 'NONE',  ( 0.000000000000000000, -1.000000000000000000, 0.000000000000000000 ) ) ;
#17829 = ORIENTED_EDGE ( 'NONE', *, *, #5834, .F. ) ;
#17830 = DIRECTION ( 'NONE',  ( 0.000000000000000000, 0.000000000000000000, -1.000000000000000000 ) ) ;
#17831 = CIRCLE ( 'NONE', #11719, 65.24900000006525147 ) ;
#17832 = CARTESIAN_POINT ( 'NONE',  ( 2.163825119083639534E-09, 18.00000000000000000, 20.95230000018031546 ) ) ;
#17833 = DIRECTION ( 'NONE',  ( -0.000000000000000000, 0.000000000000000000, -1.000000000000000000 ) ) ;
#17834 = ORIENTED_EDGE ( 'NONE', *, *, #15614, .T. ) ;
#17835 = CARTESIAN_POINT ( 'NONE',  ( -24.99999999999999289, -127.3290820621008379, -85.00000000000000000 ) ) ;
#17836 = AXIS2_PLACEMENT_3D ( 'NONE', #4755, #9643, #1494 ) ;
#17837 = ORIENTED_EDGE ( 'NONE', *, *, #18699, .F. ) ;
#17838 = CIRCLE ( 'NONE', #3918, 2.500000000000000444 ) ;
#17839 = DIRECTION ( 'NONE',  ( 0.000000000000000000, 0.000000000000000000, 1.000000000000000000 ) ) ;
#17840 = CARTESIAN_POINT ( 'NONE',  ( -31.75000000000000000, 0.000000000000000000, 0.000000000000000000 ) ) ;
#17841 = ADVANCED_FACE ( 'NONE', ( #9907 ), #10121, .T. ) ;
#17842 = ORIENTED_EDGE ( 'NONE', *, *, #20622, .F. ) ;
#17843 = ORIENTED_EDGE ( 'NONE', *, *, #5155, .F. ) ;
#17844 = DIRECTION ( 'NONE',  ( -0.000000000000000000, -0.000000000000000000, 1.000000000000000000 ) ) ;
#17845 = VECTOR ( 'NONE', #19717, 1000.000000000000000 ) ;
#17846 = DIRECTION ( 'NONE',  ( 0.000000000000000000, 0.000000000000000000, -1.000000000000000000 ) ) ;
#17847 = CONICAL_SURFACE ( 'NONE', #20539, 2.060000000000000941, 0.9599310885968777018 ) ;
#17848 = AXIS2_PLACEMENT_3D ( 'NONE', #5584, #3684, #13550 ) ;
#17849 = LINE ( 'NONE', #11264, #1506 ) ;
#17850 = VERTEX_POINT ( 'NONE', #3542 ) ;
#17851 = VECTOR ( 'NONE', #14923, 1000.000000000000000 ) ;
#17852 = CARTESIAN_POINT ( 'NONE',  ( 6.358192988180013216, 4.248408729364577141, 18.34020625018030870 ) ) ;
#17853 = AXIS2_PLACEMENT_3D ( 'NONE', #19398, #4991, #19704 ) ;
#17854 = PLANE ( 'NONE',  #5765 ) ;
#17855 = CARTESIAN_POINT ( 'NONE',  ( 19.99999999999999645, 0.000000000000000000, 0.000000000000000000 ) ) ;
#17856 = DIRECTION ( 'NONE',  ( 1.000000000000000000, 0.000000000000000000, 0.000000000000000000 ) ) ;
#17857 = ORIENTED_EDGE ( 'NONE', *, *, #14798, .F. ) ;
#17858 = DIRECTION ( 'NONE',  ( 1.000000000000000000, 0.000000000000000000, 0.000000000000000000 ) ) ;
#17859 = CARTESIAN_POINT ( 'NONE',  ( 15.25966317163202746, 10.19618095047498407, 20.52035625018031695 ) ) ;
#17860 = DIRECTION ( 'NONE',  ( 1.000000000000000000, 0.000000000000000000, 0.000000000000000000 ) ) ;
#17861 = CIRCLE ( 'NONE', #3957, 5.000000000000004441 ) ;
#17862 = ORIENTED_EDGE ( 'NONE', *, *, #3571, .F. ) ;
#17863 = CYLINDRICAL_SURFACE ( 'NONE', #11613, 27.60000000002759890 ) ;
#17864 = VERTEX_POINT ( 'NONE', #14691 ) ;
#17865 = DIRECTION ( 'NONE',  ( 1.000000000000000000, -0.000000000000000000, -0.000000000000000000 ) ) ;
#17866 = EDGE_CURVE ( 'NONE', #19846, #9320, #6931, .T. ) ;
#17867 = VECTOR ( 'NONE', #15013, 1000.000000000000000 ) ;
#17868 = VERTEX_POINT ( 'NONE', #5034 ) ;
#17869 = AXIS2_PLACEMENT_3D ( 'NONE', #17530, #12436, #17422 ) ;
#17870 = AXIS2_PLACEMENT_3D ( 'NONE', #2545, #1566, #3138 ) ;
#17871 = CARTESIAN_POINT ( 'NONE',  ( -44.00000000000000000, -85.00000000000000000, -1.040949779275250179E-14 ) ) ;
#17872 = DIRECTION ( 'NONE',  ( 0.000000000000000000, 0.000000000000000000, 1.000000000000000000 ) ) ;
#17873 = CIRCLE ( 'NONE', #7661, 27.60000000002760245 ) ;
#17874 = CARTESIAN_POINT ( 'NONE',  ( -8.382925371439629458, -12.54593441562640876, -18.71986433115845827 ) ) ;
#17875 = ORIENTED_EDGE ( 'NONE', *, *, #4093, .F. ) ;
#17876 = CARTESIAN_POINT ( 'NONE',  ( -2.271448787322325728E-15, -4.618802153517061804, -5.599999999999999645 ) ) ;
#17877 = ORIENTED_EDGE ( 'NONE', *, *, #16005, .F. ) ;
#17878 = DIRECTION ( 'NONE',  ( -1.000000000000000000, 0.000000000000000000, -0.000000000000000000 ) ) ;
#17879 = AXIS2_PLACEMENT_3D ( 'NONE', #13023, #11735, #4957 ) ;
#17880 = DIRECTION ( 'NONE',  ( -1.000000000000000000, -0.000000000000000000, -0.000000000000000000 ) ) ;
#17881 = CARTESIAN_POINT ( 'NONE',  ( 0.000000000000000000, -8.857208570070312703, 71.45313048675083678 ) ) ;
#17882 = CARTESIAN_POINT ( 'NONE',  ( 0.000000000000000000, 0.000000000000000000, 0.000000000000000000 ) ) ;
#17883 = VERTEX_POINT ( 'NONE', #8214 ) ;
#17884 = FACE_OUTER_BOUND ( 'NONE', #12956, .T. ) ;
#17885 = B_SPLINE_CURVE_WITH_KNOTS ( 'NONE', 3,
 ( #2030, #6898, #4794, #19309, #17738, #3211 ),
 .UNSPECIFIED., .F., .F.,
 ( 4, 2, 4 ),
 ( 0.006456566858647416578, 0.007625406818786683791, 0.008794246778925951871 ),
 .UNSPECIFIED. ) ;
#17886 = ORIENTED_EDGE ( 'NONE', *, *, #18415, .F. ) ;
#17887 = CARTESIAN_POINT ( 'NONE',  ( -19.21120049922023298, -12.66361362969373872, -81.30997835302029841 ) ) ;
#17888 = CARTESIAN_POINT ( 'NONE',  ( 19.99999999999999645, -67.51707036274432028, 25.00890260772354878 ) ) ;
#17889 = CARTESIAN_POINT ( 'NONE',  ( 54.64999999999999858, -39.99999999999999289, 0.000000000000000000 ) ) ;
#17890 = ORIENTED_EDGE ( 'NONE', *, *, #5532, .T. ) ;
#17891 = CARTESIAN_POINT ( 'NONE',  ( -24.99999999999999289, -170.8299878242309546, -15.48896927112552824 ) ) ;
#17892 = EDGE_CURVE ( 'NONE', #3529, #1354, #6819, .T. ) ;
#17893 = ADVANCED_FACE ( 'NONE', ( #19649 ), #18077, .F. ) ;
#17894 = CARTESIAN_POINT ( 'NONE',  ( -44.00000000000000000, -85.00000000000000000, -14.50000000000000533 ) ) ;
#17895 = APPLICATION_PROTOCOL_DEFINITION ( 'draft international standard', 'automotive_design', 1998, #11155 ) ;
#17896 = CARTESIAN_POINT ( 'NONE',  ( 6.888301780572508193, -16.62983158603122291, -22.04926249981969377 ) ) ;
#17897 = ORIENTED_EDGE ( 'NONE', *, *, #861, .T. ) ;
#17898 = CARTESIAN_POINT ( 'NONE',  ( 9.015937996181835182E-10, 7.500000000000002665, 7.442550000180307990 ) ) ;
#17899 = EDGE_CURVE ( 'NONE', #17615, #232, #1080, .T. ) ;
#17900 = DIRECTION ( 'NONE',  ( -1.000000000000000000, -0.000000000000000000, 0.000000000000000000 ) ) ;
#17901 = CARTESIAN_POINT ( 'NONE',  ( 8.382925368423265411, -12.54593441764187034, 2.169864331519073097 ) ) ;
#17902 = CYLINDRICAL_SURFACE ( 'NONE', #20391, 72.00000000007199219 ) ;
#17903 = AXIS2_PLACEMENT_3D ( 'NONE', #10931, #19201, #4681 ) ;
#17904 = VERTEX_POINT ( 'NONE', #59 ) ;
#17905 = CARTESIAN_POINT ( 'NONE',  ( -2.099999999999999645, 2.571758278209440971E-16, -5.294516984716111097 ) ) ;
#17906 = CARTESIAN_POINT ( 'NONE',  ( -7.500000000000007994, -4.022542210876018231E-17, 20.77620000000231570 ) ) ;
#17907 = CARTESIAN_POINT ( 'NONE',  ( 45.22159793441012710, -8.673994507468377080, 78.07221698934969822 ) ) ;
#17908 = VERTEX_POINT ( 'NONE', #8416 ) ;
#17909 = EDGE_CURVE ( 'NONE', #10293, #16773, #3702, .T. ) ;
#17910 = DIRECTION ( 'NONE',  ( -1.000000000000000000, 0.000000000000000000, 0.000000000000000000 ) ) ;
#17911 = ORIENTED_EDGE ( 'NONE', *, *, #8798, .F. ) ;
#17912 = DIRECTION ( 'NONE',  ( 0.000000000000000000, 0.000000000000000000, -1.000000000000000000 ) ) ;
#17913 = CARTESIAN_POINT ( 'NONE',  ( 19.99999999999999645, 64.79224928664392280, -2.456263514197840614 ) ) ;
#17914 = ORIENTED_EDGE ( 'NONE', *, *, #19914, .T. ) ;
#17915 = ORIENTED_EDGE ( 'NONE', *, *, #4167, .F. ) ;
#17916 = DIRECTION ( 'NONE',  ( 0.000000000000000000, -0.8878852184023794392, 0.4600650377311439887 ) ) ;
#17917 = ADVANCED_FACE ( 'NONE', ( #6515 ), #14891, .T. ) ;
#17918 = EDGE_CURVE ( 'NONE', #2235, #9794, #859, .T. ) ;
#17919 = DIRECTION ( 'NONE',  ( 0.000000000000000000, 0.000000000000000000, 1.000000000000000000 ) ) ;
#17920 = CARTESIAN_POINT ( 'NONE',  ( -6.679999999999997051, -11.49999999999998934, 1.408343819019455584E-15 ) ) ;
#17922 = EDGE_CURVE ( 'NONE', #20752, #1213, #8386, .T. ) ;
#17921 = DIRECTION ( 'NONE',  ( 0.000000000000000000, 0.9976687691905394839, -0.06824241336466768670 ) ) ;
#17923 = CARTESIAN_POINT ( 'NONE',  ( -7.499999999820669672, 1.491842756249032620, 11.64573125018031519 ) ) ;
#17924 = CARTESIAN_POINT ( 'NONE',  ( 7.902369978624323110, 7.902369976724394895, -1.233234750286801296 ) ) ;
#17925 = CARTESIAN_POINT ( 'NONE',  ( 0.000000000000000000, 0.000000000000000000, 3.469446951953614189E-15 ) ) ;
#17926 = CARTESIAN_POINT ( 'NONE',  ( 0.000000000000000000, 0.000000000000000000, 40.00000000000000000 ) ) ;
#17927 = EDGE_LOOP ( 'NONE', ( #15276, #1700, #8622, #14377 ) ) ;
#17928 = LINE ( 'NONE', #6156, #14965 ) ;
#17929 = CARTESIAN_POINT ( 'NONE',  ( -6.888301780572501976, 16.62983158603122291, 20.36323750018031475 ) ) ;
#17930 = DIRECTION ( 'NONE',  ( 1.000000000000000000, 0.000000000000000000, 0.000000000000000000 ) ) ;
#17931 = ORIENTED_EDGE ( 'NONE', *, *, #2742, .F. ) ;
#17932 = EDGE_CURVE ( 'NONE', #10000, #1316, #16792, .T. ) ;
#17933 = CARTESIAN_POINT ( 'NONE',  ( 19.99999999999999645, -63.85430960833482317, 16.34407078397855528 ) ) ;
#17934 = ORIENTED_EDGE ( 'NONE', *, *, #16745, .F. ) ;
#17935 = DIRECTION ( 'NONE',  ( -1.000000000000000000, -0.000000000000000000, -0.000000000000000000 ) ) ;
#17936 = CARTESIAN_POINT ( 'NONE',  ( 30.11828614405466809, -45.99142187292924433, 71.48965128677856740 ) ) ;
#17937 = EDGE_LOOP ( 'NONE', ( #6982, #13545, #12162, #3375 ) ) ;
#17938 = ORIENTED_EDGE ( 'NONE', *, *, #1398, .T. ) ;
#17939 = CARTESIAN_POINT ( 'NONE',  ( 6.250000000000054179, 10.82531754730546147, 46.00000000000000711 ) ) ;
#17940 = EDGE_CURVE ( 'NONE', #15306, #8783, #5398, .T. ) ;
#17941 = DIRECTION ( 'NONE',  ( -1.000000000000000000, -0.000000000000000000, -0.000000000000000000 ) ) ;
#17942 = LINE ( 'NONE', #9680, #1818 ) ;
#17943 = ORIENTED_EDGE ( 'NONE', *, *, #820, .T. ) ;
#17944 = CYLINDRICAL_SURFACE ( 'NONE', #3235, 27.60000000002759890 ) ;
#17945 = CARTESIAN_POINT ( 'NONE',  ( 5.303300858261588147, -5.303300859536636658, -1.608174999819685702 ) ) ;
#17946 = LINE ( 'NONE', #11270, #149 ) ;
#17947 = LINE ( 'NONE', #16155, #1155 ) ;
#17948 = ORIENTED_EDGE ( 'NONE', *, *, #601, .T. ) ;
#17949 = CARTESIAN_POINT ( 'NONE',  ( -17.50000000000000355, 0.000000000000000000, 46.00000000000000711 ) ) ;
#17950 = ORIENTED_EDGE ( 'NONE', *, *, #19395, .F. ) ;
#17951 = DIRECTION ( 'NONE',  ( 0.000000000000000000, 0.2697967711570248284, -0.9629172873477992445 ) ) ;
#17952 = DIRECTION ( 'NONE',  ( 1.000000000000000000, 0.000000000000000000, 0.000000000000000000 ) ) ;
#17953 = CIRCLE ( 'NONE', #1381, 7.500000000000000000 ) ;
#17954 = EDGE_LOOP ( 'NONE', ( #15643, #4965, #13369, #18087 ) ) ;
#17955 = DIRECTION ( 'NONE',  ( 6.938893903907228378E-17, -1.000000000000000000, 0.000000000000000000 ) ) ;
#17956 = ORIENTED_EDGE ( 'NONE', *, *, #1587, .F. ) ;
#17957 = FACE_OUTER_BOUND ( 'NONE', #3500, .T. ) ;
#17958 = ORIENTED_EDGE ( 'NONE', *, *, #16101, .T. ) ;
#17959 = VECTOR ( 'NONE', #9879, 1000.000000000000114 ) ;
#17960 = DIRECTION ( 'NONE',  ( 0.000000000000000000, -0.000000000000000000, -1.000000000000000000 ) ) ;
#17961 = CARTESIAN_POINT ( 'NONE',  ( -24.99999999999999289, -113.2094389508847314, -74.86138894033631175 ) ) ;
#17962 = CIRCLE ( 'NONE', #10867, 72.00000000007199219 ) ;
#17963 = CARTESIAN_POINT ( 'NONE',  ( 8.382925368423272516, -12.54593441764187745, -20.48705183115845685 ) ) ;
#17964 = EDGE_CURVE ( 'NONE', #17979, #714, #8118, .T. ) ;
#17965 = ORIENTED_EDGE ( 'NONE', *, *, #6858, .F. ) ;
#17966 = CARTESIAN_POINT ( 'NONE',  ( -12.50000000000000533, 0.000000000000000000, -40.00000000000000000 ) ) ;
#17967 = EDGE_CURVE ( 'NONE', #8219, #9551, #5730, .T. ) ;
#17968 = DIRECTION ( 'NONE',  ( 0.000000000000000000, 0.000000000000000000, 1.000000000000000000 ) ) ;
#17969 = ORIENTED_EDGE ( 'NONE', *, *, #10367, .T. ) ;
#17970 = CARTESIAN_POINT ( 'NONE',  ( -21.45900938229203447, -1.326995226329880762, -84.99999999999998579 ) ) ;
#17971 = EDGE_LOOP ( 'NONE', ( #10241, #19795, #19924, #19505 ) ) ;
#17972 = CARTESIAN_POINT ( 'NONE',  ( -12.72792206288791128, -12.72792205982779912, 17.41792500018031475 ) ) ;
#17973 = AXIS2_PLACEMENT_3D ( 'NONE', #11905, #5543, #5241 ) ;
#17974 = CARTESIAN_POINT ( 'NONE',  ( 0.000000000000000000, 0.000000000000000000, 169.0000000000000000 ) ) ;
#17975 = DIRECTION ( 'NONE',  ( 0.000000000000000000, -0.9422609221188166240, -0.3348796121709969320 ) ) ;
#17976 = ORIENTED_EDGE ( 'NONE', *, *, #20074, .T. ) ;
#17977 = FACE_BOUND ( 'NONE', #15285, .T. ) ;
#17978 = AXIS2_PLACEMENT_3D ( 'NONE', #1389, #4560, #9327 ) ;
#17979 = VERTEX_POINT ( 'NONE', #12348 ) ;
#17980 = PLANE ( 'NONE',  #13059 ) ;
#17981 = ORIENTED_EDGE ( 'NONE', *, *, #9228, .T. ) ;
#17982 = EDGE_CURVE ( 'NONE', #18338, #20337, #17548, .T. ) ;
#17983 = CARTESIAN_POINT ( 'NONE',  ( 2.500000000000000000, 2.357898499370433054, -1.951563910473907981E-15 ) ) ;
#17984 = DIRECTION ( 'NONE',  ( -0.000000000000000000, 0.7812527682501551052, 0.6242147964454779485 ) ) ;
#17985 = CARTESIAN_POINT ( 'NONE',  ( 2.163825119083639947E-09, 18.00000000000000355, -16.74769999981969093 ) ) ;
#17987 = ORIENTED_EDGE ( 'NONE', *, *, #4414, .F. ) ;
#17986 = AXIS2_PLACEMENT_3D ( 'NONE', #7885, #14367, #1739 ) ;
#17988 = CARTESIAN_POINT ( 'NONE',  ( -6.929096493489627306, 2.870125743571138699, 5.675362500180308523 ) ) ;
#17989 = AXIS2_PLACEMENT_3D ( 'NONE', #13653, #5580, #8555 ) ;
#17990 = CARTESIAN_POINT ( 'NONE',  ( 19.99999999999999645, -60.35829202194859278, -24.78524934717612282 ) ) ;
#17991 = CARTESIAN_POINT ( 'NONE',  ( -14.79893867758296544, 1.779018419858780125E-09, -13.44029191848092708 ) ) ;
#17992 = CARTESIAN_POINT ( 'NONE',  ( 17.50000000000000355, 0.000000000000000000, 169.0000000000000000 ) ) ;
#17993 = EDGE_CURVE ( 'NONE', #15420, #742, #4732, .T. ) ;
#17994 = ORIENTED_EDGE ( 'NONE', *, *, #12746, .T. ) ;
#17995 = DIRECTION ( 'NONE',  ( -0.000000000000000000, -0.000000000000000000, 1.000000000000000000 ) ) ;
#17996 = DIRECTION ( 'NONE',  ( 1.000000000000000000, 0.000000000000000000, 0.000000000000000000 ) ) ;
#17997 = CARTESIAN_POINT ( 'NONE',  ( 31.90258477071211729, -34.42335243099921627, 66.95649890984037711 ) ) ;
#17998 = EDGE_LOOP ( 'NONE', ( #19232, #12009, #7069, #14323, #12671, #7349, #11374, #7688, #13725, #4395, #9425, #7986, #7994, #16768, #8423, #18241, #15230, #7990, #12723, #15481 ) ) ;
#17999 = VECTOR ( 'NONE', #13624, 1000.000000000000000 ) ;
#18000 = DIRECTION ( 'NONE',  ( -1.000000000000000000, 0.000000000000000000, 0.000000000000000000 ) ) ;
#18001 = CIRCLE ( 'NONE', #1760, 0.2500000000000002220 ) ;
#18002 = ORIENTED_EDGE ( 'NONE', *, *, #12338, .F. ) ;
#18003 = CARTESIAN_POINT ( 'NONE',  ( 19.99999999999999645, 56.63599015375715595, -31.56633360682406675 ) ) ;
#18004 = CARTESIAN_POINT ( 'NONE',  ( 2.163825119083639120E-09, 17.99999999999999645, 19.04770000018030984 ) ) ;
#18005 = ORIENTED_EDGE ( 'NONE', *, *, #5847, .T. ) ;
#18006 = CIRCLE ( 'NONE', #5134, 3.199999999999994404 ) ;
#18007 = ORIENTED_EDGE ( 'NONE', *, *, #14519, .T. ) ;
#18008 = CARTESIAN_POINT ( 'NONE',  ( 19.99999999999999645, 63.85430960833475211, 11.25592921604948948 ) ) ;
#18009 = EDGE_CURVE ( 'NONE', #1571, #6843, #9377, .T. ) ;
#18010 = FACE_OUTER_BOUND ( 'NONE', #9526, .T. ) ;
#18011 = DIRECTION ( 'NONE',  ( 0.000000000000000000, -0.6310879443260434263, -0.7757112907044274586 ) ) ;
#18012 =( LENGTH_UNIT ( ) NAMED_UNIT ( * ) SI_UNIT ( .MILLI., .METRE. ) );
#18013 = CARTESIAN_POINT ( 'NONE',  ( -2.870125743571144028, -6.929096493489630859, 9.584012500180316252 ) ) ;
#18014 = VECTOR ( 'NONE', #11957, 1000.000000000000000 ) ;
#18015 = CIRCLE ( 'NONE', #6496, 2.649999999999999467 ) ;
#18016 = CARTESIAN_POINT ( 'NONE',  ( -4.276731812588563386, 10.32494394809438987, 6.424577749713199282 ) ) ;
#18017 = CIRCLE ( 'NONE', #8871, 2.649999999999993694 ) ;
#18018 = CARTESIAN_POINT ( 'NONE',  ( -52.49999999999999289, -130.0000000000000000, 5.000000000000000000 ) ) ;
#18019 = DIRECTION ( 'NONE',  ( 0.000000000000000000, 0.000000000000000000, -1.000000000000000000 ) ) ;
#18020 = EDGE_CURVE ( 'NONE', #19132, #13515, #8577, .T. ) ;
#18021 = VERTEX_POINT ( 'NONE', #20600 ) ;
#18022 = DIRECTION ( 'NONE',  ( 1.000000000000000000, 0.000000000000000000, 0.000000000000000000 ) ) ;
#18023 = EDGE_CURVE ( 'NONE', #5556, #8714, #7566, .T. ) ;
#18024 = CARTESIAN_POINT ( 'NONE',  ( 15.25966317163202746, 10.19618095047498407, 22.42495625018031191 ) ) ;
#18025 = CARTESIAN_POINT ( 'NONE',  ( 0.000000000000000000, 14.55863677812212131, -63.60407295269091321 ) ) ;
#18026 = CIRCLE ( 'NONE', #4198, 2.099999999999999645 ) ;
#18027 = ORIENTED_EDGE ( 'NONE', *, *, #19581, .F. ) ;
#18028 = CARTESIAN_POINT ( 'NONE',  ( 4.000000000000000000, 0.000000000000000000, 0.000000000000000000 ) ) ;
#18029 = EDGE_LOOP ( 'NONE', ( #747, #2091, #18847, #959, #17706 ) ) ;
#18030 = DIRECTION ( 'NONE',  ( -1.000000000000000000, -0.000000000000000000, -0.000000000000000000 ) ) ;
#18031 = CARTESIAN_POINT ( 'NONE',  ( 19.99999999999999645, 63.85430960833475211, 11.25592921604948948 ) ) ;
#18032 = ADVANCED_FACE ( 'NONE', ( #10762 ), #17224, .T. ) ;
#18033 = ORIENTED_EDGE ( 'NONE', *, *, #10637, .F. ) ;
#18034 = ORIENTED_EDGE ( 'NONE', *, *, #355, .T. ) ;
#18035 = FACE_OUTER_BOUND ( 'NONE', #2387, .T. ) ;
#18036 = AXIS2_PLACEMENT_3D ( 'NONE', #20081, #7050, #7469 ) ;
#18037 = CIRCLE ( 'NONE', #8886, 72.00000000007199219 ) ;
#18038 = AXIS2_PLACEMENT_3D ( 'NONE', #13246, #19698, #17921 ) ;
#18039 = AXIS2_PLACEMENT_3D ( 'NONE', #400, #6853, #16406 ) ;
#18040 = FACE_OUTER_BOUND ( 'NONE', #19565, .T. ) ;
#18041 = CARTESIAN_POINT ( 'NONE',  ( 40.00000000000000000, -122.3205080756887639, 86.97287527660684248 ) ) ;
#18042 = EDGE_CURVE ( 'NONE', #3964, #1999, #12553, .T. ) ;
#18043 = ORIENTED_EDGE ( 'NONE', *, *, #3165, .F. ) ;
#18044 = EDGE_CURVE ( 'NONE', #3604, #17345, #7991, .T. ) ;
#18045 = CARTESIAN_POINT ( 'NONE',  ( 6.999999999999997335, 10.52400000000000091, 0.000000000000000000 ) ) ;
#18046 = DIRECTION ( 'NONE',  ( 1.000000000000000000, 0.000000000000000000, 0.000000000000000000 ) ) ;
#18047 = DIRECTION ( 'NONE',  ( -1.000000000000000000, -0.000000000000000000, -0.000000000000000000 ) ) ;
#18048 = AXIS2_PLACEMENT_3D ( 'NONE', #1855, #17872, #3231 ) ;
#18049 = CYLINDRICAL_SURFACE ( 'NONE', #5551, 7.500000000000000000 ) ;
#18050 = CARTESIAN_POINT ( 'NONE',  ( -62.49999999999999289, -30.00000000000000000, 5.000000000000000000 ) ) ;
#18051 = CIRCLE ( 'NONE', #457, 2.649999999999999467 ) ;
#18052 = ORIENTED_EDGE ( 'NONE', *, *, #1989, .T. ) ;
#18053 = CYLINDRICAL_SURFACE ( 'NONE', #15625, 11.49999999999999467 ) ;
#18054 = EDGE_CURVE ( 'NONE', #4546, #10611, #7575, .T. ) ;
#18055 = ORIENTED_EDGE ( 'NONE', *, *, #17020, .F. ) ;
#18056 = CARTESIAN_POINT ( 'NONE',  ( 8.500000000000000000, 1.040949779275250140E-15, -90.00000000000000000 ) ) ;
#18057 = CARTESIAN_POINT ( 'NONE',  ( 0.000000000000000000, 0.000000000000000000, -0.3080913168122707546 ) ) ;
#18058 = VERTEX_POINT ( 'NONE', #18812 ) ;
#18059 = DIRECTION ( 'NONE',  ( -1.000000000000000000, -0.000000000000000000, -0.000000000000000000 ) ) ;
#18060 = ORIENTED_EDGE ( 'NONE', *, *, #976, .T. ) ;
#18061 = CARTESIAN_POINT ( 'NONE',  ( -30.00000000000000000, -85.00000000000000000, -1.040949779275250179E-14 ) ) ;
#18062 = DIRECTION ( 'NONE',  ( 0.000000000000000000, -0.5000000000000012212, -0.8660254037844380415 ) ) ;
#18063 = EDGE_CURVE ( 'NONE', #14211, #9434, #15618, .T. ) ;
#18064 = CIRCLE ( 'NONE', #4518, 80.00000000000000000 ) ;
#18065 = EDGE_LOOP ( 'NONE', ( #12378, #1351, #744, #7198 ) ) ;
#18066 = CIRCLE ( 'NONE', #3487, 27.60000000002759890 ) ;
#18067 = DIRECTION ( 'NONE',  ( 0.000000000000000000, 0.000000000000000000, 1.000000000000000000 ) ) ;
#18068 =( LENGTH_UNIT ( ) NAMED_UNIT ( * ) SI_UNIT ( .MILLI., .METRE. ) );
#18069 = VECTOR ( 'NONE', #15599, 1000.000000000000000 ) ;
#18070 = CARTESIAN_POINT ( 'NONE',  ( 50.00000000000000000, -3.649167310370807105, -90.00000000000000000 ) ) ;
#18071 = CARTESIAN_POINT ( 'NONE',  ( -1.343452921478824119E-09, -11.17563879731705789, 9.423859750647428868 ) ) ;
#18072 = ORIENTED_EDGE ( 'NONE', *, *, #4302, .F. ) ;
#18073 = CARTESIAN_POINT ( 'NONE',  ( 9.999999999999998224, 63.48283426024899256, -33.96954156735303343 ) ) ;
#18074 = CYLINDRICAL_SURFACE ( 'NONE', #3730, 55.00000000000000711 ) ;
#18075 = ORIENTED_EDGE ( 'NONE', *, *, #12046, .F. ) ;
#18076 = CIRCLE ( 'NONE', #10967, 27.60000000002759890 ) ;
#18077 = CYLINDRICAL_SURFACE ( 'NONE', #6742, 2.649999999999994582 ) ;
#18078 = CIRCLE ( 'NONE', #20778, 2.099999999999990763 ) ;
#18079 = VERTEX_POINT ( 'NONE', #19230 ) ;
#18080 = DIRECTION ( 'NONE',  ( 0.000000000000000000, -0.6310879443260434263, -0.7757112907044274586 ) ) ;
#18081 = CARTESIAN_POINT ( 'NONE',  ( 19.99999999999999645, 0.000000000000000000, 0.000000000000000000 ) ) ;
#18082 = CARTESIAN_POINT ( 'NONE',  ( 19.99999999999999645, 0.000000000000000000, 0.000000000000000000 ) ) ;
#18083 = CIRCLE ( 'NONE', #8937, 4.000000000000000000 ) ;
#18084 = ORIENTED_EDGE ( 'NONE', *, *, #11962, .F. ) ;
#18085 = VECTOR ( 'NONE', #7684, 1000.000000000000000 ) ;
#18086 = DIRECTION ( 'NONE',  ( 0.000000000000000000, -0.5195839500354404450, 0.8544194045464843512 ) ) ;
#18087 = ORIENTED_EDGE ( 'NONE', *, *, #7843, .T. ) ;
#18088 = CARTESIAN_POINT ( 'NONE',  ( 30.00000000000000000, -151.4095880458873467, -44.60680010464253087 ) ) ;
#18089 = EDGE_CURVE ( 'NONE', #20282, #19655, #9605, .T. ) ;
#18090 = AXIS2_PLACEMENT_3D ( 'NONE', #12770, #19221, #11159 ) ;
#18091 = ORIENTED_EDGE ( 'NONE', *, *, #16065, .F. ) ;
#18092 = CARTESIAN_POINT ( 'NONE',  ( 7.500000000000000000, 9.184850993605147944E-16, 46.00000000000000711 ) ) ;
#18093 = CARTESIAN_POINT ( 'NONE',  ( 50.00000000000000000, 4.299168419249266293, -84.99999999999998579 ) ) ;
#18094 = SHAPE_DEFINITION_REPRESENTATION ( #352, #20346 ) ;
#18095 = CARTESIAN_POINT ( 'NONE',  ( -13.67243654778936168, -5.663308646854336992, 19.86372941884154741 ) ) ;
#18096 = ORIENTED_EDGE ( 'NONE', *, *, #274, .T. ) ;
#18097 = CARTESIAN_POINT ( 'NONE',  ( 2.870125743571138255, 6.929096493489627306, 8.031612500180308700 ) ) ;
#18098 = VERTEX_POINT ( 'NONE', #19130 ) ;
#18099 = DIRECTION ( 'NONE',  ( 0.000000000000000000, 0.000000000000000000, 1.000000000000000000 ) ) ;
#18100 = CARTESIAN_POINT ( 'NONE',  ( -13.67243654642775041, 5.663308650141531508, -3.426229418480926991 ) ) ;
#18101 = LINE ( 'NONE', #8239, #5490 ) ;
#18102 = AXIS2_PLACEMENT_3D ( 'NONE', #16097, #9627, #6228 ) ;
#18103 = EDGE_LOOP ( 'NONE', ( #17249, #10547, #14929, #19848 ) ) ;
#18104 = FACE_OUTER_BOUND ( 'NONE', #20473, .T. ) ;
#18105 = CARTESIAN_POINT ( 'NONE',  ( 42.80822997663166518, -124.2670557317275382, -81.91943786100384273 ) ) ;
#18106 = ORIENTED_EDGE ( 'NONE', *, *, #17120, .T. ) ;
#18107 = CARTESIAN_POINT ( 'NONE',  ( -7.500000000000000000, 0.000000000000000000, 46.00000000000000711 ) ) ;
#18108 = ORIENTED_EDGE ( 'NONE', *, *, #15807, .F. ) ;
#18109 = VECTOR ( 'NONE', #15466, 1000.000000000000000 ) ;
#18110 = FACE_BOUND ( 'NONE', #10401, .T. ) ;
#18111 = CARTESIAN_POINT ( 'NONE',  ( -12.72792205982779556, 12.72792206288790773, 17.86957500018031197 ) ) ;
#18112 = EDGE_CURVE ( 'NONE', #4659, #14903, #11169, .T. ) ;
#18113 = EDGE_LOOP ( 'NONE', ( #17618, #16906, #6498, #8761 ) ) ;
#18114 = ORIENTED_EDGE ( 'NONE', *, *, #17750, .F. ) ;
#18115 = CARTESIAN_POINT ( 'NONE',  ( 19.99999999999999645, 60.35829202194909016, -24.78524934717487227 ) ) ;
#18116 = CARTESIAN_POINT ( 'NONE',  ( 0.000000000000000000, 0.000000000000000000, 0.000000000000000000 ) ) ;
#18117 = FACE_OUTER_BOUND ( 'NONE', #4816, .T. ) ;
#18118 = PRODUCT_DEFINITION_FORMATION_WITH_SPECIFIED_SOURCE ( 'ANY', '', #8811, .NOT_KNOWN. ) ;
#18119 = DIRECTION ( 'NONE',  ( -1.000000000000000000, 0.000000000000000000, 0.000000000000000000 ) ) ;
#18120 = EDGE_CURVE ( 'NONE', #9908, #7786, #6878, .T. ) ;
#18121 = CARTESIAN_POINT ( 'NONE',  ( 0.000000000000000000, -70.68211945903179583, -13.71269443944282607 ) ) ;
#18122 = CARTESIAN_POINT ( 'NONE',  ( -7.500000000179346316, -1.491842754445844355, 11.05666875018031625 ) ) ;
#18123 = AXIS2_PLACEMENT_3D ( 'NONE', #1419, #7873, #20487 ) ;
#18124 = CARTESIAN_POINT ( 'NONE',  ( 9.474249098604504482, 6.330490856366291830, 8.486296499713199992 ) ) ;
#18125 = PRODUCT_DEFINITION_SHAPE ( 'NONE', 'NONE',  #20880 ) ;
#18126 = CARTESIAN_POINT ( 'NONE',  ( -2.000000000000009770, 3.464101615137749057, -5.600000000000000533 ) ) ;
#18127 = LINE ( 'NONE', #15154, #16774 ) ;
#18128 = ORIENTED_EDGE ( 'NONE', *, *, #2503, .F. ) ;
#18129 = CARTESIAN_POINT ( 'NONE',  ( 9.999999999999998224, 0.9548212943375489203, -71.99366858485714715 ) ) ;
#18130 = CARTESIAN_POINT ( 'NONE',  ( -6.888301784570738384, -16.62983158437509346, 7.403862500180314221 ) ) ;
#18131 = DIRECTION ( 'NONE',  ( -0.000000000000000000, -0.000000000000000000, 1.000000000000000000 ) ) ;
#18132 = EDGE_LOOP ( 'NONE', ( #19241, #2289, #2152, #9790 ) ) ;
#18133 = CARTESIAN_POINT ( 'NONE',  ( 50.00000000000000000, -127.3290820621008947, -85.00000000000000000 ) ) ;
#18134 = ORIENTED_EDGE ( 'NONE', *, *, #2780, .F. ) ;
#18135 = CARTESIAN_POINT ( 'NONE',  ( 0.000000000000000000, 0.000000000000000000, 0.000000000000000000 ) ) ;
#18136 = CARTESIAN_POINT ( 'NONE',  ( 30.00000000000000000, -113.2094389508847314, 74.86138894033629754 ) ) ;
#18137 = AXIS2_PLACEMENT_3D ( 'NONE', #15970, #4947, #5042 ) ;
#18138 = ORIENTED_EDGE ( 'NONE', *, *, #7506, .F. ) ;
#18139 = EDGE_LOOP ( 'NONE', ( #20789, #768, #14931, #12837 ) ) ;
#18140 = CARTESIAN_POINT ( 'NONE',  ( 0.000000000000000000, 0.000000000000000000, 0.000000000000000000 ) ) ;
#18141 = CARTESIAN_POINT ( 'NONE',  ( 0.000000000000000000, 35.35772184876879720, 54.34979580218204376 ) ) ;
#18142 = EDGE_CURVE ( 'NONE', #17904, #16972, #17640, .T. ) ;
#18143 = EDGE_CURVE ( 'NONE', #6196, #10244, #19419, .T. ) ;
#18144 = CARTESIAN_POINT ( 'NONE',  ( 3.599999999999909051, -10.82531754730554496, 43.00000000000000000 ) ) ;
#18145 = CARTESIAN_POINT ( 'NONE',  ( -7.500000000000000888, 9.015942588607330751E-10, 5.086300000180312253 ) ) ;
#18146 = AXIS2_PLACEMENT_3D ( 'NONE', #19826, #4901, #333 ) ;
#18147 = CARTESIAN_POINT ( 'NONE',  ( 35.67727064648033064, -118.9655047900900371, -84.00146531284171658 ) ) ;
#18148 = EDGE_CURVE ( 'NONE', #10026, #13763, #471, .T. ) ;
#18149 = DIRECTION ( 'NONE',  ( 1.000000000000000000, 0.000000000000000000, 0.000000000000000000 ) ) ;
#18150 = LINE ( 'NONE', #16763, #4766 ) ;
#18151 = CARTESIAN_POINT ( 'NONE',  ( 0.000000000000000000, 0.000000000000000000, 166.0000000000000000 ) ) ;
#18152 = CIRCLE ( 'NONE', #6304, 11.49999999999999467 ) ;
#18153 = CIRCLE ( 'NONE', #20856, 4.000000000000000000 ) ;
#18154 = ORIENTED_EDGE ( 'NONE', *, *, #15854, .F. ) ;
#18155 = DIRECTION ( 'NONE',  ( 1.000000000000000000, 0.000000000000000000, 0.000000000000000000 ) ) ;
#18156 = ORIENTED_EDGE ( 'NONE', *, *, #14218, .F. ) ;
#18157 = CARTESIAN_POINT ( 'NONE',  ( -6.679999999999997939, 5.204170427930421283E-15, 0.000000000000000000 ) ) ;
#18158 = CARTESIAN_POINT ( 'NONE',  ( 0.2500000000000002220, 5.204748896376250699E-16, -4.250000000000000000 ) ) ;
#18159 = EDGE_LOOP ( 'NONE', ( #5896, #17834, #16411, #5082, #14800 ) ) ;
#18160 = FACE_OUTER_BOUND ( 'NONE', #20094, .T. ) ;
#18161 = VERTEX_POINT ( 'NONE', #5874 ) ;
#18162 = CARTESIAN_POINT ( 'NONE',  ( 2.500000000000000000, 0.000000000000000000, 0.000000000000000000 ) ) ;
#18163 = DIRECTION ( 'NONE',  ( 0.000000000000000000, -7.039457583666959814E-15, 1.000000000000000000 ) ) ;
#18164 = CIRCLE ( 'NONE', #15118, 21.50000000000000000 ) ;
#18165 = ORIENTED_EDGE ( 'NONE', *, *, #4017, .T. ) ;
#18166 = ADVANCED_FACE ( 'NONE', ( #14251 ), #4386, .F. ) ;
#18167 = CIRCLE ( 'NONE', #18857, 2.099999999999997868 ) ;
#18168 = DIRECTION ( 'NONE',  ( 1.000000000000000000, 0.000000000000000000, 0.000000000000000000 ) ) ;
#18169 = CYLINDRICAL_SURFACE ( 'NONE', #5466, 72.00000000007199219 ) ;
#18170 = EDGE_CURVE ( 'NONE', #10552, #11331, #1648, .T. ) ;
#18171 = AXIS2_PLACEMENT_3D ( 'NONE', #13138, #20861, #19585 ) ;
#18172 = MECHANICAL_DESIGN_GEOMETRIC_PRESENTATION_REPRESENTATION (  '', ( #10737 ), #4632 ) ;
#18173 = EDGE_CURVE ( 'NONE', #5471, #8014, #8394, .T. ) ;
#18174 = CARTESIAN_POINT ( 'NONE',  ( -30.00000000000000000, -85.00000000000000000, -1.040949779275250179E-14 ) ) ;
#18175 = CARTESIAN_POINT ( 'NONE',  ( -11.17563879758428769, -2.222972768810840272, 11.48557850064743135 ) ) ;
#18176 = ORIENTED_EDGE ( 'NONE', *, *, #4734, .F. ) ;
#18178 = ADVANCED_FACE ( 'NONE', ( #11476 ), #16450, .F. ) ;
#18177 = CARTESIAN_POINT ( 'NONE',  ( 6.165579999999999394, 0.000000000000000000, 10.79377999999999993 ) ) ;
#18179 = CARTESIAN_POINT ( 'NONE',  ( 19.99999999999999645, 64.44931368725519860, 10.18420179740629727 ) ) ;
#18180 = VERTEX_POINT ( 'NONE', #3413 ) ;
#18181 = AXIS2_PLACEMENT_3D ( 'NONE', #1889, #1495, #19181 ) ;
#18182 = CYLINDRICAL_SURFACE ( 'NONE', #3378, 34.99999999999999289 ) ;
#18183 = ORIENTED_EDGE ( 'NONE', *, *, #14858, .T. ) ;
#18184 = AXIS2_PLACEMENT_3D ( 'NONE', #1577, #6426, #12910 ) ;
#18185 = CARTESIAN_POINT ( 'NONE',  ( 18.00000000043041126, 3.580422610670019434, 4.164018750180312090 ) ) ;
#18186 = LINE ( 'NONE', #489, #20513 ) ;
#18187 = DIRECTION ( 'NONE',  ( -1.000000000000000000, -0.000000000000000000, -0.000000000000000000 ) ) ;
#18188 = VERTEX_POINT ( 'NONE', #5217 ) ;
#18189 = AXIS2_PLACEMENT_3D ( 'NONE', #14099, #15672, #11195 ) ;
#18190 = FACE_BOUND ( 'NONE', #7542, .T. ) ;
#18191 = ORIENTED_EDGE ( 'NONE', *, *, #8962, .T. ) ;
#18192 = CARTESIAN_POINT ( 'NONE',  ( 6.359999999999997655, 7.000462221625649605E-15, 0.000000000000000000 ) ) ;
#18193 = EDGE_CURVE ( 'NONE', #1859, #16021, #19440, .T. ) ;
#18194 = AXIS2_PLACEMENT_3D ( 'NONE', #6107, #9189, #10686 ) ;
#18195 = ORIENTED_EDGE ( 'NONE', *, *, #14885, .F. ) ;
#18196 = DIRECTION ( 'NONE',  ( 0.000000000000000000, -0.9422609221188166240, -0.3348796121709969320 ) ) ;
#18197 = CIRCLE ( 'NONE', #16175, 21.50000000000000000 ) ;
#18198 = ADVANCED_FACE ( 'NONE', ( #14762 ), #18049, .T. ) ;
#18199 = DIRECTION ( 'NONE',  ( -1.000000000000000000, 0.000000000000000000, 0.000000000000000000 ) ) ;
#18200 = APPLICATION_PROTOCOL_DEFINITION ( 'draft international standard', 'automotive_design', 1998, #12520 ) ;
#18201 = CARTESIAN_POINT ( 'NONE',  ( -1.779019326032424922E-09, -14.79893867758297610, 18.09654191884154883 ) ) ;
#18203 = EDGE_LOOP ( 'NONE', ( #9098, #17602 ) ) ;
#18202 = AXIS2_PLACEMENT_3D ( 'NONE', #20854, #1281, #12605 ) ;
#18204 = CARTESIAN_POINT ( 'NONE',  ( 21.50000000000000000, 2.632990618166809235E-15, -84.99999999999998579 ) ) ;
#18205 = DIRECTION ( 'NONE',  ( -1.000000000000000000, -0.000000000000000000, -0.000000000000000000 ) ) ;
#18206 = CARTESIAN_POINT ( 'NONE',  ( -8.382925368423267187, 12.54593441764186856, -21.39263566848092424 ) ) ;
#18207 = EDGE_CURVE ( 'NONE', #18964, #4085, #14566, .T. ) ;
#18208 = DIRECTION ( 'NONE',  ( -1.000000000000000000, 0.000000000000000000, 0.000000000000000000 ) ) ;
#18209 =( REPRESENTATION_RELATIONSHIP ('NONE','NONE', #13739, #20346 ) REPRESENTATION_RELATIONSHIP_WITH_TRANSFORMATION ( #8851 )SHAPE_REPRESENTATION_RELATIONSHIP( ) );
#18210 = EDGE_LOOP ( 'NONE', ( #12472, #11156, #15809, #4201 ) ) ;
#18211 = CARTESIAN_POINT ( 'NONE',  ( 31.01315681530222079, -111.3007080733049889, 79.47988500914458143 ) ) ;
#18212 = CARTESIAN_POINT ( 'NONE',  ( -6.358192987158592047, 4.248408730893246776, 15.39489375018031048 ) ) ;
#18213 = VERTEX_POINT ( 'NONE', #16249 ) ;
#18214 = DIRECTION ( 'NONE',  ( 0.000000000000000000, 0.000000000000000000, 1.000000000000000000 ) ) ;
#18215 = EDGE_LOOP ( 'NONE', ( #5843, #17115, #8268, #15263 ) ) ;
#18216 = CYLINDRICAL_SURFACE ( 'NONE', #13258, 65.24900000006525147 ) ;
#18217 = CARTESIAN_POINT ( 'NONE',  ( 18.00000000043040771, 3.580422610670018546, 11.68441875018030984 ) ) ;
#18218 = EDGE_LOOP ( 'NONE', ( #18340, #1923, #9040, #8956 ) ) ;
#18219 = ORIENTED_EDGE ( 'NONE', *, *, #15312, .T. ) ;
#18220 = FACE_OUTER_BOUND ( 'NONE', #13733, .T. ) ;
#18221 = DIRECTION ( 'NONE',  ( 0.000000000000000000, 0.000000000000000000, 1.000000000000000000 ) ) ;
#18222 = DIRECTION ( 'NONE',  ( 0.000000000000000000, 0.000000000000000000, 1.000000000000000000 ) ) ;
#18223 = CARTESIAN_POINT ( 'NONE',  ( 12.72792206288791128, 12.72792205982780267, 22.13042500018031333 ) ) ;
#18224 = B_SPLINE_CURVE_WITH_KNOTS ( 'NONE', 3,
 ( #18460, #3715, #17085, #20139, #6904, #15177 ),
 .UNSPECIFIED., .F., .F.,
 ( 4, 2, 4 ),
 ( 0.006456566858647417445, 0.007625406818786684658, 0.008794246778925951871 ),
 .UNSPECIFIED. ) ;
#18225 = CARTESIAN_POINT ( 'NONE',  ( 19.99999999999999645, 0.9548212943375593564, -71.99366858485714715 ) ) ;
#18226 = CARTESIAN_POINT ( 'NONE',  ( 2.870125743571140475, 6.929096493489632635, 4.871512500180315008 ) ) ;
#18227 = EDGE_CURVE ( 'NONE', #16021, #5613, #3857, .T. ) ;
#18228 = CARTESIAN_POINT ( 'NONE',  ( 11.17563879731704723, -1.343450868547281106E-09, -18.90510975028680818 ) ) ;
#18229 = EDGE_CURVE ( 'NONE', #10611, #7712, #9784, .T. ) ;
#18230 = LINE ( 'NONE', #11858, #15810 ) ;
#18231 = FACE_OUTER_BOUND ( 'NONE', #13202, .T. ) ;
#18232 = ORIENTED_EDGE ( 'NONE', *, *, #7137, .F. ) ;
#18233 = DIRECTION ( 'NONE',  ( -1.000000000000000000, -0.000000000000000000, 0.000000000000000000 ) ) ;
#18234 = CARTESIAN_POINT ( 'NONE',  ( -18.00000000000000000, 2.163826221265758884E-09, -9.678949999819687733 ) ) ;
#18235 = CARTESIAN_POINT ( 'NONE',  ( 19.99999999999999645, 0.000000000000000000, 0.000000000000000000 ) ) ;
#18236 = ORIENTED_EDGE ( 'NONE', *, *, #11662, .F. ) ;
#18237 = CARTESIAN_POINT ( 'NONE',  ( 6.679999999999998828, 11.17999999999999972, 0.000000000000000000 ) ) ;
#18238 = ORIENTED_EDGE ( 'NONE', *, *, #11250, .T. ) ;
#18239 = PLANE ( 'NONE',  #6467 ) ;
#18240 = DIRECTION ( 'NONE',  ( 1.000000000000000000, 0.000000000000000000, 0.000000000000000000 ) ) ;
#18241 = ORIENTED_EDGE ( 'NONE', *, *, #12825, .T. ) ;
#18242 = ORIENTED_EDGE ( 'NONE', *, *, #14776, .F. ) ;
#18243 = CARTESIAN_POINT ( 'NONE',  ( 19.99999999999999645, 20.34307325858786086, 69.06634035770315450 ) ) ;
#18244 = SHAPE_REPRESENTATION_RELATIONSHIP ( 'NONE' , 'NONE' ,  #4392, #3656 ) ;
#18245 = DIRECTION ( 'NONE',  ( -0.7071067811865369146, 8.659560562355062281E-17, -0.7071067811865582309 ) ) ;
#18246 = DIRECTION ( 'NONE',  ( 0.000000000000000000, 0.000000000000000000, 1.000000000000000000 ) ) ;
#18247 = CARTESIAN_POINT ( 'NONE',  ( 37.20644374907093521, -120.3958613208574207, -85.16797049535011865 ) ) ;
#18248 = DIRECTION ( 'NONE',  ( 0.000000000000000000, 0.000000000000000000, 1.000000000000000000 ) ) ;
#18249 = DIRECTION ( 'NONE',  ( -0.000000000000000000, -0.000000000000000000, -1.000000000000000000 ) ) ;
#18250 = DIRECTION ( 'NONE',  ( -1.000000000000000000, 0.000000000000000000, 0.000000000000000000 ) ) ;
#18251 = ORIENTED_EDGE ( 'NONE', *, *, #12921, .F. ) ;
#18252 = CARTESIAN_POINT ( 'NONE',  ( 19.99999999999999645, -36.59093685910670501, 62.00889726308018624 ) ) ;
#18253 = ORIENTED_EDGE ( 'NONE', *, *, #6726, .F. ) ;
#18254 = CARTESIAN_POINT ( 'NONE',  ( 16.62983158603122291, 6.888301780572502864, 20.81488750018031553 ) ) ;
#18255 = CARTESIAN_POINT ( 'NONE',  ( -0.8281006575391447466, -21.49753944123813909, 70.58133206268971094 ) ) ;
#18256 = EDGE_CURVE ( 'NONE', #12996, #5196, #7592, .T. ) ;
#18257 = VERTEX_POINT ( 'NONE', #4804 ) ;
#18258 = EDGE_CURVE ( 'NONE', #12350, #7632, #8487, .T. ) ;
#18259 = DIRECTION ( 'NONE',  ( 0.000000000000000000, 0.1361666490962400722, 0.9906859460363316439 ) ) ;
#18260 = EDGE_LOOP ( 'NONE', ( #3364, #7388, #14442, #8010 ) ) ;
#18261 = CARTESIAN_POINT ( 'NONE',  ( 18.00000000000000000, -2.163824016901520184E-09, -24.76874999981969339 ) ) ;
#18262 = DIRECTION ( 'NONE',  ( 0.000000000000000000, 0.000000000000000000, -1.000000000000000000 ) ) ;
#18263 = EDGE_CURVE ( 'NONE', #19902, #13263, #17946, .T. ) ;
#18264 = ORIENTED_EDGE ( 'NONE', *, *, #9637, .F. ) ;
#18265 = DIRECTION ( 'NONE',  ( 0.000000000000000000, 0.000000000000000000, -1.000000000000000000 ) ) ;
#18266 = CARTESIAN_POINT ( 'NONE',  ( -16.62983158437509701, 6.888301784570728614, -1.569487499819690379 ) ) ;
#18267 =( LENGTH_UNIT ( ) NAMED_UNIT ( * ) SI_UNIT ( .MILLI., .METRE. ) );
#18268 = EDGE_CURVE ( 'NONE', #16309, #2973, #6567, .T. ) ;
#18269 = CARTESIAN_POINT ( 'NONE',  ( 6.249999999999902300, -10.82531754730554496, 43.00000000000000000 ) ) ;
#18270 = CARTESIAN_POINT ( 'NONE',  ( -2.222972768810837607, 11.17563879758428769, 13.84182850064743064 ) ) ;
#18271 = EDGE_LOOP ( 'NONE', ( #3488, #17026, #7615, #12574 ) ) ;
#18272 = CARTESIAN_POINT ( 'NONE',  ( 30.00000000000000000, -99.99999999999998579, -54.09999999999998721 ) ) ;
#18273 = DIRECTION ( 'NONE',  ( -1.000000000000000000, 0.000000000000000000, 0.000000000000000000 ) ) ;
#18274 = ORIENTED_EDGE ( 'NONE', *, *, #5468, .T. ) ;
#18275 = CARTESIAN_POINT ( 'NONE',  ( -7.539743116613892404, -20.19060691129837792, -71.13878616268860355 ) ) ;
#18276 = VERTEX_POINT ( 'NONE', #3217 ) ;
#18277 = CARTESIAN_POINT ( 'NONE',  ( -10.19618095047498052, 15.25966317163203101, 1.218706250180313866 ) ) ;
#18278 = DIRECTION ( 'NONE',  ( -1.000000000000000000, 0.000000000000000000, -0.000000000000000000 ) ) ;
#18279 = CARTESIAN_POINT ( 'NONE',  ( -6.359999999999997655, 4.663913298532544267E-15, 0.000000000000000000 ) ) ;
#18280 = ADVANCED_FACE ( 'NONE', ( #6699 ), #1839, .F. ) ;
#18281 = ORIENTED_EDGE ( 'NONE', *, *, #8747, .T. ) ;
#18282 = EDGE_CURVE ( 'NONE', #9123, #15726, #10094, .T. ) ;
#18283 = AXIS2_PLACEMENT_3D ( 'NONE', #17637, #16248, #8094 ) ;
#18284 = DIRECTION ( 'NONE',  ( -1.000000000000000000, 0.000000000000000000, 0.000000000000000000 ) ) ;
#18285 = ORIENTED_EDGE ( 'NONE', *, *, #4033, .F. ) ;
#18286 = DIRECTION ( 'NONE',  ( -1.000000000000000000, -0.000000000000000000, -0.000000000000000000 ) ) ;
#18287 = EDGE_CURVE ( 'NONE', #9780, #18021, #17761, .T. ) ;
#18288 = VECTOR ( 'NONE', #11487, 1000.000000000000000 ) ;
#18289 = ORIENTED_EDGE ( 'NONE', *, *, #4511, .T. ) ;
#18290 = DIRECTION ( 'NONE',  ( -0.000000000000000000, -0.000000000000000000, 1.000000000000000000 ) ) ;
#18291 = PRODUCT_DEFINITION_SHAPE ( 'NONE', 'NONE',  #20952 ) ;
#18292 = DIRECTION ( 'NONE',  ( 0.000000000000000000, 0.000000000000000000, 1.000000000000000000 ) ) ;
#18293 = CARTESIAN_POINT ( 'NONE',  ( 14.79893867722910450, -2.943691928843438443, 16.03482316884154812 ) ) ;
#18294 = ORIENTED_EDGE ( 'NONE', *, *, #7435, .F. ) ;
#18295 = CIRCLE ( 'NONE', #2732, 27.60000000002759535 ) ;
#18296 = CYLINDRICAL_SURFACE ( 'NONE', #17371, 65.24900000006525147 ) ;
#18297 = ORIENTED_EDGE ( 'NONE', *, *, #1323, .T. ) ;
#18298 = EDGE_CURVE ( 'NONE', #11336, #14260, #13278, .T. ) ;
#18299 = EDGE_CURVE ( 'NONE', #13448, #12949, #4886, .T. ) ;
#18300 = CARTESIAN_POINT ( 'NONE',  ( 10.46442989202483531, -10.46442989454075168, -26.39966691848093561 ) ) ;
#18301 = VECTOR ( 'NONE', #6052, 1000.000000000000114 ) ;
#18302 = CARTESIAN_POINT ( 'NONE',  ( 30.00000000000000000, -170.8299878242309546, 15.48896927112552824 ) ) ;
#18303 = VECTOR ( 'NONE', #13264, 1000.000000000000000 ) ;
#18304 = ORIENTED_EDGE ( 'NONE', *, *, #1222, .T. ) ;
#18305 = EDGE_CURVE ( 'NONE', #14577, #14343, #18150, .T. ) ;
#18306 = CARTESIAN_POINT ( 'NONE',  ( 39.62815566457561545, -122.1058236485348374, 86.75687390987235403 ) ) ;
#18307 = CARTESIAN_POINT ( 'NONE',  ( -5.303300858261584594, 5.303300859536631329, 15.68942500018031083 ) ) ;
#18308 = ORIENTED_EDGE ( 'NONE', *, *, #20095, .T. ) ;
#18309 = CARTESIAN_POINT ( 'NONE',  ( -6.929096494179684207, -2.870125741905212635, 10.76213750018031590 ) ) ;
#18310 = VERTEX_POINT ( 'NONE', #15074 ) ;
#18311 = DIRECTION ( 'NONE',  ( -0.000000000000000000, -0.000000000000000000, -1.000000000000000000 ) ) ;
#18312 = CARTESIAN_POINT ( 'NONE',  ( 10.19618095047497697, -15.25966317163202923, 13.45160625018031197 ) ) ;
#18313 = EDGE_LOOP ( 'NONE', ( #14080, #2773, #6408 ) ) ;
#18314 = ORIENTED_EDGE ( 'NONE', *, *, #5893, .T. ) ;
#18315 = CARTESIAN_POINT ( 'NONE',  ( 6.249999999999902300, -10.82531754730554496, 126.0000000000000000 ) ) ;
#18316 = AXIS2_PLACEMENT_3D ( 'NONE', #11498, #1969, #14499 ) ;
#18317 = DIRECTION ( 'NONE',  ( -1.000000000000000000, -0.000000000000000000, -0.000000000000000000 ) ) ;
#18318 = DIRECTION ( 'NONE',  ( 1.836909530733573776E-16, -1.000000000000000000, 0.000000000000000000 ) ) ;
#18319 = CIRCLE ( 'NONE', #19011, 18.00000000000000000 ) ;
#18320 = CARTESIAN_POINT ( 'NONE',  ( -7.500000000000009770, 9.706494107251932559E-15, -16.92379999999768359 ) ) ;
#18321 = UNCERTAINTY_MEASURE_WITH_UNIT (LENGTH_MEASURE( 1.000000000000000082E-05 ), #13661, 'distance_accuracy_value', 'NONE');
#18322 = LINE ( 'NONE', #3033, #12011 ) ;
#18323 = CARTESIAN_POINT ( 'NONE',  ( 7.500000000179346316, 1.491842754445843244, -3.080831249819684814 ) ) ;
#18324 = APPLICATION_CONTEXT ( 'automotive_design' ) ;
#18325 = CIRCLE ( 'NONE', #3431, 27.60000000002759535 ) ;
#18326 = CARTESIAN_POINT ( 'NONE',  ( 9.474249097082495297, -6.330490858644137298, -18.02151600028679823 ) ) ;
#18327 = CARTESIAN_POINT ( 'NONE',  ( 19.99999999999999645, 68.15657073222435258, 23.20952102120304517 ) ) ;
#18328 = CARTESIAN_POINT ( 'NONE',  ( 9.999999999999998224, 63.48283426024851650, 33.96954156735390740 ) ) ;
#18329 = AXIS2_PLACEMENT_3D ( 'NONE', #19329, #12681, #9280 ) ;
#18330 = VECTOR ( 'NONE', #10098, 1000.000000000000000 ) ;
#18331 = ORIENTED_EDGE ( 'NONE', *, *, #1858, .F. ) ;
#18332 = DIRECTION ( 'NONE',  ( 0.000000000000000000, 0.000000000000000000, 1.000000000000000000 ) ) ;
#18333 = CARTESIAN_POINT ( 'NONE',  ( 15.25966316918061416, -10.19618095414378622, 5.342143750180314399 ) ) ;
#18334 = CARTESIAN_POINT ( 'NONE',  ( -12.50000000000000533, 0.000000000000000000, 43.00000000000000000 ) ) ;
#18335 = CIRCLE ( 'NONE', #6809, 11.50000000000000000 ) ;
#18336 = ORIENTED_EDGE ( 'NONE', *, *, #5963, .F. ) ;
#18337 = DIRECTION ( 'NONE',  ( 0.000000000000000000, 0.000000000000000000, -1.000000000000000000 ) ) ;
#18338 = VERTEX_POINT ( 'NONE', #15386 ) ;
#18339 = FACE_OUTER_BOUND ( 'NONE', #18945, .T. ) ;
#18340 = ORIENTED_EDGE ( 'NONE', *, *, #15985, .T. ) ;
#18341 = VERTEX_POINT ( 'NONE', #18670 ) ;
#18342 = DIRECTION ( 'NONE',  ( 0.000000000000000000, 0.000000000000000000, 1.000000000000000000 ) ) ;
#18343 = EDGE_CURVE ( 'NONE', #11771, #12132, #16655, .T. ) ;
#18344 = SURFACE_SIDE_STYLE ('',( #13065 ) ) ;
#18345 = CARTESIAN_POINT ( 'NONE',  ( 19.99999999999999645, -56.63599015375651646, -31.56633360682521072 ) ) ;
#18346 = CIRCLE ( 'NONE', #12591, 2.649999999999988365 ) ;
#18347 = VECTOR ( 'NONE', #849, 1000.000000000000000 ) ;
#18348 = CARTESIAN_POINT ( 'NONE',  ( 40.00000000000000711, -30.00000000000001421, -120.0000000000000142 ) ) ;
#18349 = AXIS2_PLACEMENT_3D ( 'NONE', #853, #1067, #9012 ) ;
#18350 = CARTESIAN_POINT ( 'NONE',  ( 6.929096493489624642, -2.870125743571141363, 0.9628625001803121641 ) ) ;
#18351 = CARTESIAN_POINT ( 'NONE',  ( 1.040949779275250179E-14, -85.00000000000000000, 0.000000000000000000 ) ) ;
#18352 = CARTESIAN_POINT ( 'NONE',  ( 0.000000000000000000, 60.35829202194909016, -24.78524934717487227 ) ) ;
#18353 = CARTESIAN_POINT ( 'NONE',  ( 2.500000000000000000, 2.357898499370433054, -1.951563910473907981E-15 ) ) ;
#18354 = LINE ( 'NONE', #12107, #3173 ) ;
#18355 = VERTEX_POINT ( 'NONE', #18353 ) ;
#18356 = VERTEX_POINT ( 'NONE', #12200 ) ;
#18357 = CARTESIAN_POINT ( 'NONE',  ( 12.72792206288790950, 12.72792205982780089, 10.80082500018031411 ) ) ;
#18358 = CARTESIAN_POINT ( 'NONE',  ( 19.99999999999999645, 61.72688495901586947, 19.84591825364119089 ) ) ;
#18359 = AXIS2_PLACEMENT_3D ( 'NONE', #8771, #13770, #5801 ) ;
#18360 = VERTEX_POINT ( 'NONE', #5515 ) ;
#18361 = CIRCLE ( 'NONE', #11598, 27.60000000002759890 ) ;
#18362 = DIRECTION ( 'NONE',  ( -1.000000000000000000, -0.000000000000000000, 0.000000000000000000 ) ) ;
#18363 = ORIENTED_EDGE ( 'NONE', *, *, #7266, .T. ) ;
#18364 = CARTESIAN_POINT ( 'NONE',  ( -52.49999999999999289, -30.00000000000000000, 5.000000000000000000 ) ) ;
#18365 = DIRECTION ( 'NONE',  ( -0.000000000000000000, -0.000000000000000000, -1.000000000000000000 ) ) ;
#18366 = CLOSED_SHELL ( 'NONE', ( #18166, #1066, #16227, #16735, #17893, #1285, #17058, #9480, #14921, #17424, #13214, #20382, #20662, #18178, #19947, #12728, #20889, #18778, #19738, #16664, #3919, #19659 ) ) ;
#18367 = TOROIDAL_SURFACE ( 'NONE', #2447, 2.700000000000000622, 0.2000000000000000111 ) ;
#18368 = EDGE_LOOP ( 'NONE', ( #12914, #3888, #17205, #4651 ) ) ;
#18369 = ADVANCED_FACE ( 'NONE', ( #4141 ), #10509, .F. ) ;
#18370 = AXIS2_PLACEMENT_3D ( 'NONE', #14271, #15533, #4310 ) ;
#18371 = LINE ( 'NONE', #13602, #9740 ) ;
#18372 = CARTESIAN_POINT ( 'NONE',  ( 3.580422610670019878, -18.00000000043040771, -14.23433124981968767 ) ) ;
#18373 = DIRECTION ( 'NONE',  ( -1.000000000000000000, -0.000000000000000000, -0.000000000000000000 ) ) ;
#18374 = CARTESIAN_POINT ( 'NONE',  ( 6.680000000000000604, 6.938893903907228378E-15, 0.000000000000000000 ) ) ;
#18375 = CARTESIAN_POINT ( 'NONE',  ( 1.343451552857795926E-09, 11.17563879731705789, 14.13635975064743100 ) ) ;
#18376 = CIRCLE ( 'NONE', #11924, 65.24900000006526568 ) ;
#18377 = EDGE_CURVE ( 'NONE', #4533, #20501, #18224, .T. ) ;
#18379 = ORIENTED_EDGE ( 'NONE', *, *, #15831, .F. ) ;
#18378 = AXIS2_PLACEMENT_3D ( 'NONE', #8000, #11176, #6401 ) ;
#18380 = PRESENTATION_STYLE_ASSIGNMENT (( #13930 ) ) ;
#18381 = FACE_OUTER_BOUND ( 'NONE', #1547, .T. ) ;
#18382 = EDGE_LOOP ( 'NONE', ( #13684, #10902, #11044, #14231 ) ) ;
#18383 = CARTESIAN_POINT ( 'NONE',  ( 16.80529800326410239, -13.48305675317430108, -74.69048503828150842 ) ) ;
#18384 = ORIENTED_EDGE ( 'NONE', *, *, #8570, .F. ) ;
#18385 = CARTESIAN_POINT ( 'NONE',  ( -3.580422610670018546, 18.00000000043041126, 1.807768750180311468 ) ) ;
#18386 = CARTESIAN_POINT ( 'NONE',  ( -17.50000000000000355, 0.000000000000000000, 46.00000000000000711 ) ) ;
#18387 = CARTESIAN_POINT ( 'NONE',  ( 0.000000000000000000, -51.96384592647235934, 49.83732252579597599 ) ) ;
#18388 = CIRCLE ( 'NONE', #6208, 27.60000000002760245 ) ;
#18389 = ORIENTED_EDGE ( 'NONE', *, *, #6647, .F. ) ;
#18390 = DIRECTION ( 'NONE',  ( -1.000000000000000000, 0.000000000000000000, -0.000000000000000000 ) ) ;
#18391 = EDGE_LOOP ( 'NONE', ( #9803, #1339, #3347, #3105 ) ) ;
#18392 = CARTESIAN_POINT ( 'NONE',  ( 6.929096494179683319, 2.870125741905213079, 15.47463750018031625 ) ) ;
#18393 = ORIENTED_EDGE ( 'NONE', *, *, #5026, .T. ) ;
#18394 = VECTOR ( 'NONE', #19642, 1000.000000000000000 ) ;
#18395 = FACE_OUTER_BOUND ( 'NONE', #8246, .T. ) ;
#18396 = AXIS2_PLACEMENT_3D ( 'NONE', #10635, #2781, #2576 ) ;
#18397 = VERTEX_POINT ( 'NONE', #7010 ) ;
#18398 = LINE ( 'NONE', #16913, #19525 ) ;
#18399 = CARTESIAN_POINT ( 'NONE',  ( 0.000000000000000000, 0.000000000000000000, 0.000000000000000000 ) ) ;
#18400 = SHAPE_DEFINITION_REPRESENTATION ( #18125, #9416 ) ;
#18401 = AXIS2_PLACEMENT_3D ( 'NONE', #19533, #11170, #9576 ) ;
#18402 = CARTESIAN_POINT ( 'NONE',  ( -5.663308646854337880, 13.67243654778935991, 12.79497941884154777 ) ) ;
#18403 = AXIS2_PLACEMENT_3D ( 'NONE', #11539, #1902, #18011 ) ;
#18404 = EDGE_CURVE ( 'NONE', #896, #19670, #20032, .T. ) ;
#18405 = EDGE_LOOP ( 'NONE', ( #7607, #19879, #15077, #5004 ) ) ;
#18406 = B_SPLINE_CURVE_WITH_KNOTS ( 'NONE', 3,
 ( #13784, #4234, #2748, #2428, #6035, #18766 ),
 .UNSPECIFIED., .F., .F.,
 ( 4, 2, 4 ),
 ( 0.002336974151641521731, 0.003500975885716455828, 0.004664977619791389925 ),
 .UNSPECIFIED. ) ;
#18407 = ADVANCED_FACE ( 'NONE', ( #15272 ), #2144, .F. ) ;
#18408 = DIRECTION ( 'NONE',  ( 1.000000000000000000, 0.000000000000000000, 0.000000000000000000 ) ) ;
#18409 = AXIS2_PLACEMENT_3D ( 'NONE', #19953, #5431, #11900 ) ;
#18410 = DIRECTION ( 'NONE',  ( 1.000000000000000000, 0.000000000000000000, 0.000000000000000000 ) ) ;
#18411 = CARTESIAN_POINT ( 'NONE',  ( 16.62983158603121936, 6.888301780572501976, 20.81488750018031197 ) ) ;
#18412 = AXIS2_PLACEMENT_3D ( 'NONE', #16160, #11689, #6705 ) ;
#18413 = DIRECTION ( 'NONE',  ( -1.000000000000000000, -0.000000000000000000, -0.000000000000000000 ) ) ;
#18414 = ADVANCED_FACE ( 'NONE', ( #13491 ), #12203, .T. ) ;
#18415 = EDGE_CURVE ( 'NONE', #10139, #10694, #7212, .T. ) ;
#18416 = ORIENTED_EDGE ( 'NONE', *, *, #7537, .F. ) ;
#18417 = DIRECTION ( 'NONE',  ( 0.000000000000000000, 0.000000000000000000, 1.000000000000000000 ) ) ;
#18418 = DIRECTION ( 'NONE',  ( 0.000000000000000000, 0.000000000000000000, -1.000000000000000000 ) ) ;
#18419 = CIRCLE ( 'NONE', #9955, 2.649999999999999467 ) ;
#18420 = ORIENTED_EDGE ( 'NONE', *, *, #7210, .F. ) ;
#18421 = DIRECTION ( 'NONE',  ( 1.000000000000000000, 0.000000000000000000, 0.000000000000000000 ) ) ;
#18422 = ORIENTED_EDGE ( 'NONE', *, *, #16366, .T. ) ;
#18423 = CARTESIAN_POINT ( 'NONE',  ( 50.00000000000000000, 4.299168419249259188, 90.00000000000000000 ) ) ;
#18424 = CARTESIAN_POINT ( 'NONE',  ( 3.580422614997667896, 17.99999999956958163, 0.4922312501803097207 ) ) ;
#18425 = ORIENTED_EDGE ( 'NONE', *, *, #4005, .F. ) ;
#18426 = ORIENTED_EDGE ( 'NONE', *, *, #537, .F. ) ;
#18427 = LINE ( 'NONE', #948, #2934 ) ;
#18428 = EDGE_CURVE ( 'NONE', #8932, #6625, #11882, .T. ) ;
#18429 = CIRCLE ( 'NONE', #20456, 27.60000000002759890 ) ;
#18430 = DIRECTION ( 'NONE',  ( 1.000000000000000000, 0.000000000000000000, 0.000000000000000000 ) ) ;
#18431 = DIRECTION ( 'NONE',  ( -1.000000000000000000, 0.000000000000000000, 0.000000000000000000 ) ) ;
#18432 = CARTESIAN_POINT ( 'NONE',  ( 0.000000000000000000, -58.26603306961936113, -42.29739224042532442 ) ) ;
#18433 = EDGE_CURVE ( 'NONE', #10000, #19384, #8473, .T. ) ;
#18434 = EDGE_CURVE ( 'NONE', #10469, #14887, #10305, .T. ) ;
#18435 = CARTESIAN_POINT ( 'NONE',  ( -2.870125743571144028, -6.929096493489630859, 0.1590125001803138760 ) ) ;
#18436 = CARTESIAN_POINT ( 'NONE',  ( -2.870125743571144028, -6.929096493489630859, 19.00901250018031519 ) ) ;
#18437 = CARTESIAN_POINT ( 'NONE',  ( 9.474249098604504482, 6.330490856366291830, -19.78870350028680747 ) ) ;
#18438 = EDGE_CURVE ( 'NONE', #12005, #4533, #15591, .T. ) ;
#18439 = CARTESIAN_POINT ( 'NONE',  ( -4.000000000000000000, 2.309401076758531346, -5.242734410091827613 ) ) ;
#18440 = AXIS2_PLACEMENT_3D ( 'NONE', #17661, #3236, #3131 ) ;
#18441 = VERTEX_POINT ( 'NONE', #2452 ) ;
#18442 = CARTESIAN_POINT ( 'NONE',  ( 19.99999999999999645, -20.34307325858833693, 69.06634035770301239 ) ) ;
#18443 = CARTESIAN_POINT ( 'NONE',  ( 17.99999999956958163, -3.580422614997676334, -4.671918749819689687 ) ) ;
#18444 = CYLINDRICAL_SURFACE ( 'NONE', #14808, 2.649999999999994582 ) ;
#18445 = ORIENTED_EDGE ( 'NONE', *, *, #2175, .F. ) ;
#18446 = LINE ( 'NONE', #2021, #8237 ) ;
#18447 = VERTEX_POINT ( 'NONE', #11786 ) ;
#18448 = FACE_OUTER_BOUND ( 'NONE', #18405, .T. ) ;
#18449 = DIRECTION ( 'NONE',  ( 1.000000000000000000, 0.000000000000000000, 0.000000000000000000 ) ) ;
#18450 = ORIENTED_EDGE ( 'NONE', *, *, #7668, .T. ) ;
#18451 = ORIENTED_EDGE ( 'NONE', *, *, #16576, .T. ) ;
#18452 = AXIS2_PLACEMENT_3D ( 'NONE', #6027, #17370, #12598 ) ;
#18453 = DIRECTION ( 'NONE',  ( 1.000000000000000000, 0.000000000000000000, 0.000000000000000000 ) ) ;
#18454 = ADVANCED_FACE ( 'NONE', ( #10412 ), #14971, .F. ) ;
#18455 = DIRECTION ( 'NONE',  ( 0.000000000000000000, 0.000000000000000000, 1.000000000000000000 ) ) ;
#18456 = CARTESIAN_POINT ( 'NONE',  ( 0.000000000000000000, 61.72688495901586947, 19.84591825364119089 ) ) ;
#18457 = CARTESIAN_POINT ( 'NONE',  ( -5.303300859536631329, -5.303300858261583706, -14.94182499981969237 ) ) ;
#18458 = CARTESIAN_POINT ( 'NONE',  ( 30.32391323356592139, -108.7007521017901439, -78.47408402981700704 ) ) ;
#18459 = DIRECTION ( 'NONE',  ( 0.000000000000000000, -0.9976687691905398170, 0.06824241336466072005 ) ) ;
#18460 = CARTESIAN_POINT ( 'NONE',  ( 4.000000000000000000, 0.000000000000000000, -5.600000000000000533 ) ) ;
#18461 = DIRECTION ( 'NONE',  ( -0.000000000000000000, 0.000000000000000000, -1.000000000000000000 ) ) ;
#18462 = ORIENTED_EDGE ( 'NONE', *, *, #11283, .F. ) ;
#18463 = EDGE_CURVE ( 'NONE', #19105, #1793, #12106, .T. ) ;
#18464 = DIRECTION ( 'NONE',  ( 0.000000000000000000, 1.000000000000000000, 0.000000000000000000 ) ) ;
#18465 = CIRCLE ( 'NONE', #6287, 7.567219999999999835 ) ;
#18466 = ORIENTED_EDGE ( 'NONE', *, *, #799, .F. ) ;
#18467 = CARTESIAN_POINT ( 'NONE',  ( -16.62983158437510056, 6.888301784570729502, 7.855512500180314106 ) ) ;
#18468 = CARTESIAN_POINT ( 'NONE',  ( -10.25561400234659004, -18.90011081285701877, 71.73813932909899904 ) ) ;
#18469 = VERTEX_POINT ( 'NONE', #4031 ) ;
#18470 = DIRECTION ( 'NONE',  ( 1.000000000000000000, 0.000000000000000000, 0.000000000000000000 ) ) ;
#18471 = ORIENTED_EDGE ( 'NONE', *, *, #15763, .T. ) ;
#18472 = AXIS2_PLACEMENT_3D ( 'NONE', #18671, #2568, #7427 ) ;
#18473 = PRODUCT_DEFINITION_SHAPE ( 'NONE', 'NONE',  #20969 ) ;
#18474 = CARTESIAN_POINT ( 'NONE',  ( 28.13963350654227824, -26.35784117651622793, -130.0000000000000000 ) ) ;
#18475 = DIRECTION ( 'NONE',  ( 0.000000000000000000, 0.000000000000000000, 1.000000000000000000 ) ) ;
#18476 = ORIENTED_EDGE ( 'NONE', *, *, #7534, .F. ) ;
#18477 = CARTESIAN_POINT ( 'NONE',  ( 22.70866746290765903, -3.649167310370807105, -90.00000000000000000 ) ) ;
#18478 = CARTESIAN_POINT ( 'NONE',  ( 0.000000000000000000, 49.77519642624007901, 42.18840861821802690 ) ) ;
#18479 = CARTESIAN_POINT ( 'NONE',  ( 3.580422614997667896, 17.99999999956958163, -18.35776874981969442 ) ) ;
#18480 = DIRECTION ( 'NONE',  ( 0.000000000000000000, 0.000000000000000000, 1.000000000000000000 ) ) ;
#18481 = AXIS2_PLACEMENT_3D ( 'NONE', #15980, #10801, #7930 ) ;
#18482 = CIRCLE ( 'NONE', #5280, 27.60000000002759890 ) ;
#18483 = CARTESIAN_POINT ( 'NONE',  ( 0.000000000000000000, -11.98658579560543025, -64.13855129306480762 ) ) ;
#18484 = CARTESIAN_POINT ( 'NONE',  ( 4.276731815070943910, 10.32494394706616703, 14.72542225064742993 ) ) ;
#18485 = VERTEX_POINT ( 'NONE', #16968 ) ;
#18486 = CIRCLE ( 'NONE', #17484, 27.60000000002760245 ) ;
#18487 = VECTOR ( 'NONE', #11764, 1000.000000000000000 ) ;
#18488 = CARTESIAN_POINT ( 'NONE',  ( 30.00000000000000000, -99.99999999999998579, -54.09999999999999432 ) ) ;
#18489 = CYLINDRICAL_SURFACE ( 'NONE', #27, 27.60000000002760245 ) ;
#18490 = ORIENTED_EDGE ( 'NONE', *, *, #15465, .F. ) ;
#18491 = CARTESIAN_POINT ( 'NONE',  ( -14.94551481348181809, -15.47228562136405827, -73.52041642655927944 ) ) ;
#18492 = ORIENTED_EDGE ( 'NONE', *, *, #12467, .T. ) ;
#18493 = EDGE_CURVE ( 'NONE', #1745, #8829, #13390, .T. ) ;
#18494 = CARTESIAN_POINT ( 'NONE',  ( -12.72792206288791128, -12.72792205982779912, 7.992925000180314044 ) ) ;
#18495 = AXIS2_PLACEMENT_3D ( 'NONE', #18031, #8276, #16237 ) ;
#18496 = DIRECTION ( 'NONE',  ( 0.000000000000000000, 0.000000000000000000, 1.000000000000000000 ) ) ;
#18497 = FACE_OUTER_BOUND ( 'NONE', #9960, .T. ) ;
#18498 = VERTEX_POINT ( 'NONE', #6263 ) ;
#18499 = CARTESIAN_POINT ( 'NONE',  ( 19.99999999999999645, 0.000000000000000000, 0.000000000000000000 ) ) ;
#18500 = CONICAL_SURFACE ( 'NONE', #5671, 4.000000000000000000, 1.047197551196595855 ) ;
#18501 = ORIENTED_EDGE ( 'NONE', *, *, #10108, .F. ) ;
#18502 = CARTESIAN_POINT ( 'NONE',  ( -1.491842754445842800, 7.500000000179346316, 13.41291875018031554 ) ) ;
#18503 = CIRCLE ( 'NONE', #4956, 2.649999999999987477 ) ;
#18504 = EDGE_CURVE ( 'NONE', #701, #12949, #7643, .T. ) ;
#18505 = ORIENTED_EDGE ( 'NONE', *, *, #17909, .T. ) ;
#18506 = CARTESIAN_POINT ( 'NONE',  ( 7.500000000000000888, -9.015933403756337545E-10, 19.22380000018031154 ) ) ;
#18507 = CIRCLE ( 'NONE', #5972, 17.50000000000000355 ) ;
#18508 = AXIS2_PLACEMENT_3D ( 'NONE', #18279, #10443, #5442 ) ;
#18509 = ORIENTED_EDGE ( 'NONE', *, *, #1996, .F. ) ;
#18510 = DIRECTION ( 'NONE',  ( 0.000000000000000000, -0.7308359642781161458, -0.6825531432186624503 ) ) ;
#18511 = AXIS2_PLACEMENT_3D ( 'NONE', #7549, #9459, #17310 ) ;
#18512 = DIRECTION ( 'NONE',  ( 0.000000000000000000, 0.000000000000000000, -1.000000000000000000 ) ) ;
#18513 = CARTESIAN_POINT ( 'NONE',  ( 12.54593441764187567, 8.382925368423276069, 14.85669816884154848 ) ) ;
#18514 = VERTEX_POINT ( 'NONE', #12641 ) ;
#18515 = AXIS2_PLACEMENT_3D ( 'NONE', #10891, #17366, #2728 ) ;
#18516 = FACE_OUTER_BOUND ( 'NONE', #16184, .T. ) ;
#18517 = EDGE_LOOP ( 'NONE', ( #5219, #10720, #2198, #16494 ) ) ;
#18518 = CARTESIAN_POINT ( 'NONE',  ( -5.705422232504516522, -20.77800788743411076, 76.38232661121730871 ) ) ;
#18519 = CIRCLE ( 'NONE', #240, 2.649999999999999467 ) ;
#18520 = CARTESIAN_POINT ( 'NONE',  ( -17.99999999999999645, 2.163826221265758470E-09, 16.69145000018031055 ) ) ;
#18521 = AXIS2_PLACEMENT_3D ( 'NONE', #16944, #14944, #2219 ) ;
#18522 = CARTESIAN_POINT ( 'NONE',  ( 0.000000000000000000, 20.60847369613070867, -61.90898814327694311 ) ) ;
#18523 = ORIENTED_EDGE ( 'NONE', *, *, #19316, .F. ) ;
#18524 = CARTESIAN_POINT ( 'NONE',  ( 29.99999999999999645, -105.9493285778136595, 77.66804255791004152 ) ) ;
#18525 = CARTESIAN_POINT ( 'NONE',  ( 6.929096494179677990, 2.870125741905210859, 18.63473750018030728 ) ) ;
#18526 = VECTOR ( 'NONE', #11439, 1000.000000000000000 ) ;
#18527 = ORIENTED_EDGE ( 'NONE', *, *, #18268, .F. ) ;
#18528 = EDGE_CURVE ( 'NONE', #17518, #9946, #20354, .T. ) ;
#18529 = CARTESIAN_POINT ( 'NONE',  ( 7.582106015220150930, -21.76672924613218996, -75.91315008488570015 ) ) ;
#18530 = VERTEX_POINT ( 'NONE', #14124 ) ;
#18531 = CARTESIAN_POINT ( 'NONE',  ( 0.000000000000000000, 0.000000000000000000, 81.99999999999998579 ) ) ;
#18532 = CARTESIAN_POINT ( 'NONE',  ( -15.25966317163202923, -10.19618095047497874, 6.382856250180309665 ) ) ;
#18533 = CIRCLE ( 'NONE', #2967, 65.24900000006525147 ) ;
#18534 = EDGE_CURVE ( 'NONE', #834, #9768, #2672, .T. ) ;
#18535 = VERTEX_POINT ( 'NONE', #20576 ) ;
#18536 = ORIENTED_EDGE ( 'NONE', *, *, #14459, .T. ) ;
#18537 = CARTESIAN_POINT ( 'NONE',  ( 19.99999999999999645, 64.80702306891106446, -7.581672767545749814 ) ) ;
#18538 = CIRCLE ( 'NONE', #9404, 5.000000000000004441 ) ;
#18539 = AXIS2_PLACEMENT_3D ( 'NONE', #12557, #11173, #3017 ) ;
#18540 = CARTESIAN_POINT ( 'NONE',  ( 0.000000000000000000, 29.55812890831981932, 65.65300461859698089 ) ) ;
#18541 = CARTESIAN_POINT ( 'NONE',  ( 6.232799999999998342, 0.000000000000000000, 7.567219999999999835 ) ) ;
#18542 = EDGE_CURVE ( 'NONE', #18441, #7455, #12501, .T. ) ;
#18543 =( LENGTH_UNIT ( ) NAMED_UNIT ( * ) SI_UNIT ( .MILLI., .METRE. ) );
#18544 = CARTESIAN_POINT ( 'NONE',  ( -6.929096493489632635, 2.870125743571140919, -16.33473749981968837 ) ) ;
#18545 = FACE_OUTER_BOUND ( 'NONE', #11285, .T. ) ;
#18546 = CARTESIAN_POINT ( 'NONE',  ( -1.491842754445842800, 7.500000000179346316, 3.987918750180313054 ) ) ;
#18547 = DIRECTION ( 'NONE',  ( 1.000000000000000000, 0.000000000000000000, 0.000000000000000000 ) ) ;
#18548 = CARTESIAN_POINT ( 'NONE',  ( 1.343451552857795099E-09, 11.17563879731704723, -11.83635975028680498 ) ) ;
#18549 = AXIS2_PLACEMENT_3D ( 'NONE', #18116, #5071, #12659 ) ;
#18550 = CARTESIAN_POINT ( 'NONE',  ( 19.99999999999999645, 19.38316218894295417, -61.87375713200968619 ) ) ;
#18551 = ADVANCED_FACE ( 'NONE', ( #1403 ), #15805, .T. ) ;
#18552 = ORIENTED_EDGE ( 'NONE', *, *, #4341, .F. ) ;
#18553 = DIRECTION ( 'NONE',  ( 1.000000000000000000, 0.000000000000000000, 0.000000000000000000 ) ) ;
#18554 = CARTESIAN_POINT ( 'NONE',  ( 6.888301784570728614, 16.62983158437510056, 2.691362500180312978 ) ) ;
#18555 = DIRECTION ( 'NONE',  ( 1.000000000000000000, 0.000000000000000000, 0.000000000000000000 ) ) ;
#18556 = ORIENTED_EDGE ( 'NONE', *, *, #20607, .T. ) ;
#18557 = EDGE_CURVE ( 'NONE', #6717, #20518, #16219, .T. ) ;
#18558 = DIRECTION ( 'NONE',  ( -1.000000000000000000, -0.000000000000000000, -0.000000000000000000 ) ) ;
#18559 = VERTEX_POINT ( 'NONE', #10827 ) ;
#18560 = CARTESIAN_POINT ( 'NONE',  ( 0.000000000000000000, 39.37110852956887186, -51.51683813304829584 ) ) ;
#18561 = CARTESIAN_POINT ( 'NONE',  ( -6.232800000000000118, 0.000000000000000000, 7.567219999999999835 ) ) ;
#18562 = EDGE_CURVE ( 'NONE', #11867, #1857, #13511, .T. ) ;
#18563 = ORIENTED_EDGE ( 'NONE', *, *, #4958, .F. ) ;
#18564 = ORIENTED_EDGE ( 'NONE', *, *, #8713, .T. ) ;
#18565 = DIRECTION ( 'NONE',  ( 0.000000000000000000, -0.9976687691905398170, 0.06824241336466078944 ) ) ;
#18566 = EDGE_CURVE ( 'NONE', #9811, #8208, #17223, .T. ) ;
#18567 = CARTESIAN_POINT ( 'NONE',  ( 52.50000000000000000, -130.0000000000000000, 0.000000000000000000 ) ) ;
#18568 = CARTESIAN_POINT ( 'NONE',  ( 2.000000000000027089, 3.464101615137739731, 0.000000000000000000 ) ) ;
#18569 = CARTESIAN_POINT ( 'NONE',  ( 7.500000000179339210, 1.491842754445841690, -9.345731249819689168 ) ) ;
#18570 = CARTESIAN_POINT ( 'NONE',  ( -6.679999999999997939, 5.204170427930421283E-15, 0.000000000000000000 ) ) ;
#18571 = EDGE_CURVE ( 'NONE', #12561, #1182, #20782, .T. ) ;
#18572 = CARTESIAN_POINT ( 'NONE',  ( 150.0000507999999968, 3.872983346207417021, -1.000000000000000000 ) ) ;
#18573 = DIRECTION ( 'NONE',  ( 0.000000000000000000, -1.000000000000000000, 0.000000000000000000 ) ) ;
#18574 = ADVANCED_FACE ( 'NONE', ( #12747 ), #12485, .T. ) ;
#18575 = EDGE_CURVE ( 'NONE', #1825, #9811, #1088, .T. ) ;
#18576 = ORIENTED_EDGE ( 'NONE', *, *, #10308, .T. ) ;
#18577 = CARTESIAN_POINT ( 'NONE',  ( 0.000000000000000000, 63.17103598352126426, 16.33561182745161844 ) ) ;
#18578 = ORIENTED_EDGE ( 'NONE', *, *, #6484, .T. ) ;
#18579 = CARTESIAN_POINT ( 'NONE',  ( -15.25966316918061771, 10.19618095414378622, -1.274956249819686471 ) ) ;
#18580 = CARTESIAN_POINT ( 'NONE',  ( -13.32881486730457610, -16.88549087568889107, 72.74798471664088595 ) ) ;
#18581 = ORIENTED_EDGE ( 'NONE', *, *, #12903, .F. ) ;
#18582 = CARTESIAN_POINT ( 'NONE',  ( 0.000000000000000000, 71.89099403602354244, -3.960426305689042970 ) ) ;
#18583 = ORIENTED_EDGE ( 'NONE', *, *, #954, .F. ) ;
#18584 = DIRECTION ( 'NONE',  ( -1.000000000000000000, 0.000000000000000000, 0.000000000000000000 ) ) ;
#18585 = LINE ( 'NONE', #18685, #14119 ) ;
#18586 = ADVANCED_FACE ( 'NONE', ( #2876 ), #11036, .T. ) ;
#18587 = VERTEX_POINT ( 'NONE', #11141 ) ;
#18588 = LINE ( 'NONE', #4271, #11365 ) ;
#18589 = CARTESIAN_POINT ( 'NONE',  ( 0.000000000000000000, 46.01927912072591198, -45.67597560296339765 ) ) ;
#18590 = CARTESIAN_POINT ( 'NONE',  ( -18.00000000043040771, -3.580422610670021211, -11.87808124981969016 ) ) ;
#18591 = DIRECTION ( 'NONE',  ( 1.000000000000000000, 0.000000000000000000, 0.000000000000000000 ) ) ;
#18592 = DIRECTION ( 'NONE',  ( -0.000000000000000000, -0.000000000000000000, 1.000000000000000000 ) ) ;
#18593 = CARTESIAN_POINT ( 'NONE',  ( -9.474249098604513364, -6.330490856366295382, -7.953483999352573441 ) ) ;
#18594 = ORIENTED_EDGE ( 'NONE', *, *, #13376, .T. ) ;
#18595 = SURFACE_STYLE_USAGE ( .BOTH. , #12127 ) ;
#18596 = DIRECTION ( 'NONE',  ( 0.000000000000000000, 0.8878852184023731109, 0.4600650377311559791 ) ) ;
#18597 = VERTEX_POINT ( 'NONE', #9032 ) ;
#18598 = CARTESIAN_POINT ( 'NONE',  ( 20.76542986210400343, -5.602711969362187183, -80.65560201174187682 ) ) ;
#18599 = ORIENTED_EDGE ( 'NONE', *, *, #624, .T. ) ;
#18600 = CARTESIAN_POINT ( 'NONE',  ( -16.62983158603122291, -6.888301780572501087, 8.581987500180312978 ) ) ;
#18601 = CARTESIAN_POINT ( 'NONE',  ( -4.000000000000000000, -2.309401076758531346, -0.3572655899081733644 ) ) ;
#18602 = DIRECTION ( 'NONE',  ( 1.000000000000000000, 0.000000000000000000, -0.000000000000000000 ) ) ;
#18603 = ORIENTED_EDGE ( 'NONE', *, *, #3533, .F. ) ;
#18604 = CARTESIAN_POINT ( 'NONE',  ( 50.00000000000000000, -1.326995226329893862, 84.99999999999998579 ) ) ;
#18605 = EDGE_LOOP ( 'NONE', ( #2662, #12778 ) ) ;
#18606 = CARTESIAN_POINT ( 'NONE',  ( 5.303300859536635770, 5.303300858261589923, 14.88557500018031554 ) ) ;
#18607 = EDGE_LOOP ( 'NONE', ( #15484, #13650, #6695, #19146 ) ) ;
#18608 = FACE_OUTER_BOUND ( 'NONE', #13206, .T. ) ;
#18609 = APPLICATION_CONTEXT ( 'automotive_design' ) ;
#18610 = DIRECTION ( 'NONE',  ( -1.000000000000000000, 0.000000000000000000, 0.000000000000000000 ) ) ;
#18611 = EDGE_CURVE ( 'NONE', #18597, #3682, #8007, .T. ) ;
#18612 = EDGE_CURVE ( 'NONE', #16592, #7692, #5975, .T. ) ;
#18613 = DIRECTION ( 'NONE',  ( -1.000000000000000000, 0.000000000000000000, 0.000000000000000000 ) ) ;
#18614 = CARTESIAN_POINT ( 'NONE',  ( 12.54593441764187567, 8.382925368423276069, -3.993301831158456050 ) ) ;
#18615 = VERTEX_POINT ( 'NONE', #1307 ) ;
#18616 = DIRECTION ( 'NONE',  ( -1.000000000000000000, 0.000000000000000000, 0.000000000000000000 ) ) ;
#18617 = ORIENTED_EDGE ( 'NONE', *, *, #7015, .F. ) ;
#18618 = DIRECTION ( 'NONE',  ( 0.000000000000000000, -0.3984010898462485573, 0.9172113015054500496 ) ) ;
#18619 = CARTESIAN_POINT ( 'NONE',  ( 12.54593441562639988, -8.382925371439625906, -17.26919816848092637 ) ) ;
#18620 = DIRECTION ( 'NONE',  ( 0.000000000000000000, -0.2697967711570313232, 0.9629172873477972461 ) ) ;
#18621 = VERTEX_POINT ( 'NONE', #13906 ) ;
#18622 = CARTESIAN_POINT ( 'NONE',  ( 35.37092464391603386, -118.6634975751123591, 83.76198506216627493 ) ) ;
#18623 = CARTESIAN_POINT ( 'NONE',  ( -2.000000000000022649, -3.464101615137742396, -5.600000000000000533 ) ) ;
#18624 = EDGE_LOOP ( 'NONE', ( #9326, #20070, #8558, #14816 ) ) ;
#18625 = CARTESIAN_POINT ( 'NONE',  ( -0.7189812636139246704, -23.00150371214196809, -75.37276332846732885 ) ) ;
#18626 = ORIENTED_EDGE ( 'NONE', *, *, #8396, .T. ) ;
#18627 = CARTESIAN_POINT ( 'NONE',  ( -54.64999999999999858, -99.99999999999998579, 0.000000000000000000 ) ) ;
#18628 = CARTESIAN_POINT ( 'NONE',  ( 15.25966317163202568, 10.19618095047498230, 1.670356250180308422 ) ) ;
#18629 = EDGE_LOOP ( 'NONE', ( #16044, #7441, #1056, #19282 ) ) ;
#18630 = ORIENTED_EDGE ( 'NONE', *, *, #18562, .T. ) ;
#18631 = CARTESIAN_POINT ( 'NONE',  ( 0.000000000000000000, 62.46228066917787203, 18.86519267363478036 ) ) ;
#18632 = CARTESIAN_POINT ( 'NONE',  ( 19.99999999999999645, -51.81019761368295207, -38.98425606966110735 ) ) ;
#18633 = EDGE_CURVE ( 'NONE', #13088, #5471, #13429, .T. ) ;
#18634 = AXIS2_PLACEMENT_3D ( 'NONE', #19623, #9983, #452 ) ;
#18635 = CARTESIAN_POINT ( 'NONE',  ( 30.00000000000000711, -30.00000000000001421, -130.0000000000000000 ) ) ;
#18636 = CARTESIAN_POINT ( 'NONE',  ( 19.99999999999999645, -0.9548212943370493200, 71.99366858485714715 ) ) ;
#18637 = DIRECTION ( 'NONE',  ( 0.000000000000000000, 0.000000000000000000, -1.000000000000000000 ) ) ;
#18638 = DIRECTION ( 'NONE',  ( 0.000000000000000000, 0.000000000000000000, -1.000000000000000000 ) ) ;
#18639 = CARTESIAN_POINT ( 'NONE',  ( 9.015937996181842420E-10, 7.500000000000007994, -5.142549999819685524 ) ) ;
#18640 = CIRCLE ( 'NONE', #19318, 65.24900000006526568 ) ;
#18641 = CARTESIAN_POINT ( 'NONE',  ( 20.55500000000001748, 0.000000000000000000, 0.000000000000000000 ) ) ;
#18642 = ADVANCED_FACE ( 'NONE', ( #14018, #12423 ), #9238, .F. ) ;
#18643 = CARTESIAN_POINT ( 'NONE',  ( -9.474249098604506258, -6.330490856366290053, -24.50120350028680960 ) ) ;
#18644 = PRODUCT ( 'cover', 'cover', '', ( #286 ) ) ;
#18645 = CARTESIAN_POINT ( 'NONE',  ( 21.00000000000000355, 0.000000000000000000, 0.000000000000000000 ) ) ;
#18646 = ORIENTED_EDGE ( 'NONE', *, *, #7181, .F. ) ;
#18647 = DIRECTION ( 'NONE',  ( -1.597351267013635284E-16, 1.000000000000000000, 0.000000000000000000 ) ) ;
#18648 = CARTESIAN_POINT ( 'NONE',  ( 18.00000000043041126, 3.580422610670019434, 4.164018750180312090 ) ) ;
#18649 = DIRECTION ( 'NONE',  ( 0.000000000000000000, 0.000000000000000000, -1.000000000000000000 ) ) ;
#18650 = ORIENTED_EDGE ( 'NONE', *, *, #11943, .F. ) ;
#18651 = EDGE_CURVE ( 'NONE', #18355, #5544, #6568, .T. ) ;
#18652 = DIRECTION ( 'NONE',  ( -0.000000000000000000, -0.000000000000000000, 1.000000000000000000 ) ) ;
#18653 = VERTEX_POINT ( 'NONE', #16225 ) ;
#18654 = DIRECTION ( 'NONE',  ( -1.000000000000000000, 0.000000000000000000, -0.000000000000000000 ) ) ;
#18655 = CARTESIAN_POINT ( 'NONE',  ( 37.35049175653090714, -20.28192400168857645, -71.09734905643766467 ) ) ;
#18656 = VERTEX_POINT ( 'NONE', #9547 ) ;
#18657 = AXIS2_PLACEMENT_3D ( 'NONE', #7414, #19084, #971 ) ;
#18658 = EDGE_LOOP ( 'NONE', ( #6234, #11233, #14751, #15163 ) ) ;
#18659 = DIRECTION ( 'NONE',  ( 0.000000000000000000, 0.000000000000000000, 1.000000000000000000 ) ) ;
#18660 =( NAMED_UNIT ( * ) PLANE_ANGLE_UNIT ( ) SI_UNIT ( $, .RADIAN. ) );
#18661 = LINE ( 'NONE', #10502, #7895 ) ;
#18662 = LINE ( 'NONE', #9026, #7230 ) ;
#18663 = EDGE_CURVE ( 'NONE', #15454, #988, #16895, .T. ) ;
#18664 = AXIS2_PLACEMENT_3D ( 'NONE', #8294, #12977, #13079 ) ;
#18665 = CARTESIAN_POINT ( 'NONE',  ( 2.870125743571137811, 6.929096493489625530, -1.393387499819688458 ) ) ;
#18666 = EDGE_CURVE ( 'NONE', #5687, #20286, #14843, .T. ) ;
#18667 = CARTESIAN_POINT ( 'NONE',  ( 10.00000000000000178, -160.0000000000000000, -73.20000000000000284 ) ) ;
#18668 = CIRCLE ( 'NONE', #20691, 2.649999999999987477 ) ;
#18669 = DIRECTION ( 'NONE',  ( 0.000000000000000000, 0.000000000000000000, 1.000000000000000000 ) ) ;
#18670 = CARTESIAN_POINT ( 'NONE',  ( -17.50000000000000355, 2.143131898507868643E-15, 129.0000000000000000 ) ) ;
#18671 = CARTESIAN_POINT ( 'NONE',  ( 0.000000000000000000, 0.000000000000000000, 68.00000000000000000 ) ) ;
#18672 = EDGE_LOOP ( 'NONE', ( #10968, #5262, #1260 ) ) ;
#18673 = FACE_OUTER_BOUND ( 'NONE', #5242, .T. ) ;
#18674 = ORIENTED_EDGE ( 'NONE', *, *, #10901, .F. ) ;
#18675 = EDGE_CURVE ( 'NONE', #7631, #2747, #17827, .T. ) ;
#18676 = CARTESIAN_POINT ( 'NONE',  ( 6.888301784570728614, 16.62983158437510056, 0.7867625001803136842 ) ) ;
#18677 = CARTESIAN_POINT ( 'NONE',  ( -9.249412617561585392, -19.41235462500713993, 71.49717528132291022 ) ) ;
#18678 = EDGE_CURVE ( 'NONE', #11750, #6239, #15881, .T. ) ;
#18679 = AXIS2_PLACEMENT_3D ( 'NONE', #15491, #4252, #5724 ) ;
#18680 = ORIENTED_EDGE ( 'NONE', *, *, #18825, .T. ) ;
#18681 = CARTESIAN_POINT ( 'NONE',  ( -10.00000000000000000, 0.000000000000000000, 0.000000000000000000 ) ) ;
#18682 = VERTEX_POINT ( 'NONE', #3192 ) ;
#18683 = DIRECTION ( 'NONE',  ( 0.000000000000000000, -1.000000000000000000, -8.673617379884035472E-17 ) ) ;
#18684 = CYLINDRICAL_SURFACE ( 'NONE', #19875, 65.24900000006525147 ) ;
#18685 = CARTESIAN_POINT ( 'NONE',  ( -31.74999999999995737, 0.000000000000000000, 2.500000000000000444 ) ) ;
#18686 = VERTEX_POINT ( 'NONE', #19502 ) ;
#18687 = CYLINDRICAL_SURFACE ( 'NONE', #15758, 5.000000000000004441 ) ;
#18688 = VECTOR ( 'NONE', #9989, 1000.000000000000000 ) ;
#18689 = AXIS2_PLACEMENT_3D ( 'NONE', #2551, #14000, #12512 ) ;
#18690 = EDGE_CURVE ( 'NONE', #4727, #8495, #3386, .T. ) ;
#18691 = DIRECTION ( 'NONE',  ( -1.000000000000000000, -0.000000000000000000, -0.000000000000000000 ) ) ;
#18692 = CARTESIAN_POINT ( 'NONE',  ( -3.580422610670017658, 18.00000000043040771, -0.09683124981969132294 ) ) ;
#18693 = CARTESIAN_POINT ( 'NONE',  ( -4.000000000000000000, 1.935983797701083420, -5.350530693383767300 ) ) ;
#18694 = EDGE_CURVE ( 'NONE', #7455, #9587, #2544, .T. ) ;
#18695 = CARTESIAN_POINT ( 'NONE',  ( -62.49999999999999289, -130.0000000000000000, 0.000000000000000000 ) ) ;
#18696 = CARTESIAN_POINT ( 'NONE',  ( 11.17563879704982632, -2.222972771497745637, -2.062858999352573441 ) ) ;
#18697 = VERTEX_POINT ( 'NONE', #14739 ) ;
#18698 = DIRECTION ( 'NONE',  ( 0.000000000000000000, 0.3984010898462424510, -0.9172113015054526031 ) ) ;
#18699 = EDGE_CURVE ( 'NONE', #6196, #12585, #13154, .T. ) ;
#18700 = CYLINDRICAL_SURFACE ( 'NONE', #5084, 3.199999999999994404 ) ;
#18701 = ORIENTED_EDGE ( 'NONE', *, *, #152, .F. ) ;
#18702 = AXIS2_PLACEMENT_3D ( 'NONE', #12820, #12911, #15772 ) ;
#18703 = CARTESIAN_POINT ( 'NONE',  ( 7.575000000000064126, 13.12028486733421850, -43.00000000000000000 ) ) ;
#18704 = VECTOR ( 'NONE', #5393, 1000.000000000000000 ) ;
#18705 = ORIENTED_EDGE ( 'NONE', *, *, #175, .T. ) ;
#18706 = AXIS2_PLACEMENT_3D ( 'NONE', #3460, #8345, #14822 ) ;
#18707 = CARTESIAN_POINT ( 'NONE',  ( 16.62983158603122291, 6.888301780572502864, -5.555512499819688088 ) ) ;
#18708 = CIRCLE ( 'NONE', #5833, 27.60000000002759890 ) ;
#18709 = DIRECTION ( 'NONE',  ( 0.000000000000000000, 0.000000000000000000, -1.000000000000000000 ) ) ;
#18710 = CARTESIAN_POINT ( 'NONE',  ( 2.060000000000000941, 0.000000000000000000, -0.3080913168122707546 ) ) ;
#18711 = ORIENTED_EDGE ( 'NONE', *, *, #19521, .F. ) ;
#18712 = LINE ( 'NONE', #2606, #5850 ) ;
#18713 = ORIENTED_EDGE ( 'NONE', *, *, #5690, .T. ) ;
#18714 = CARTESIAN_POINT ( 'NONE',  ( 8.899999999999890221, -10.82531754730554496, 166.0000000000000000 ) ) ;
#18715 = EDGE_LOOP ( 'NONE', ( #16430, #15474, #9938, #7970 ) ) ;
#18716 = FACE_OUTER_BOUND ( 'NONE', #7128, .T. ) ;
#18717 = CIRCLE ( 'NONE', #2133, 39.99999999999999289 ) ;
#18718 = CIRCLE ( 'NONE', #19373, 65.24900000006525147 ) ;
#18719 = EDGE_CURVE ( 'NONE', #8465, #19301, #9761, .T. ) ;
#18720 = STYLED_ITEM ( 'NONE', ( #416 ), #10194 ) ;
#18721 = LINE ( 'NONE', #5773, #8206 ) ;
#18722 = MECHANICAL_DESIGN_GEOMETRIC_PRESENTATION_REPRESENTATION (  '', ( #2468 ), #5856 ) ;
#18723 = CARTESIAN_POINT ( 'NONE',  ( 13.67243654778935991, 5.663308646854338768, -3.698770581158455695 ) ) ;
#18724 = EDGE_LOOP ( 'NONE', ( #14392, #12787, #14696, #8732 ) ) ;
#18725 = DIRECTION ( 'NONE',  ( -1.000000000000000000, 0.000000000000000000, 0.000000000000000000 ) ) ;
#18726 = ORIENTED_EDGE ( 'NONE', *, *, #2227, .T. ) ;
#18727 = AXIS2_PLACEMENT_3D ( 'NONE', #3353, #6328, #9620 ) ;
#18728 = CARTESIAN_POINT ( 'NONE',  ( -20.21355047154532159, -7.393864663665485004, 85.82585403120822320 ) ) ;
#18729 = VECTOR ( 'NONE', #18245, 1000.000000000000000 ) ;
#18730 = CARTESIAN_POINT ( 'NONE',  ( 10.19618095047497697, -15.25966317163202923, 4.026606250180309488 ) ) ;
#18731 = CARTESIAN_POINT ( 'NONE',  ( 0.000000000000000000, 0.000000000000000000, -40.00000000000000000 ) ) ;
#18732 = CARTESIAN_POINT ( 'NONE',  ( 85.00002539999999840, 5.400000000000000355, 1.000000000000000000 ) ) ;
#18733 = AXIS2_PLACEMENT_3D ( 'NONE', #2925, #5235, #6505 ) ;
#18734 = VECTOR ( 'NONE', #1847, 1000.000000000000000 ) ;
#18735 = ORIENTED_EDGE ( 'NONE', *, *, #18229, .F. ) ;
#18736 = ADVANCED_FACE ( 'NONE', ( #7966 ), #14540, .T. ) ;
#18737 = FACE_OUTER_BOUND ( 'NONE', #17335, .T. ) ;
#18738 = FACE_BOUND ( 'NONE', #1912, .T. ) ;
#18739 = APPLICATION_CONTEXT ( 'automotive_design' ) ;
#18740 = ORIENTED_EDGE ( 'NONE', *, *, #5387, .F. ) ;
#18741 = CARTESIAN_POINT ( 'NONE',  ( 16.48273624093881651, -16.04508369211728436, -78.99984814018115742 ) ) ;
#18742 = ORIENTED_EDGE ( 'NONE', *, *, #20724, .T. ) ;
#18743 = CARTESIAN_POINT ( 'NONE',  ( -1.491842756249031954, -7.499999999820663454, 3.024581250180308434 ) ) ;
#18744 = CARTESIAN_POINT ( 'NONE',  ( -6.888301780572500199, 16.62983158603121936, -9.816362499819691223 ) ) ;
#18745 = VERTEX_POINT ( 'NONE', #7 ) ;
#18746 = CIRCLE ( 'NONE', #18401, 27.60000000002760245 ) ;
#18747 = ORIENTED_EDGE ( 'NONE', *, *, #15037, .F. ) ;
#18748 = CYLINDRICAL_SURFACE ( 'NONE', #2279, 14.49999999999999467 ) ;
#18749 = CIRCLE ( 'NONE', #19099, 2.649999999999999467 ) ;
#18750 = VECTOR ( 'NONE', #16551, 1000.000000000000000 ) ;
#18751 = DIRECTION ( 'NONE',  ( 1.000000000000000000, 0.000000000000000000, 0.000000000000000000 ) ) ;
#18752 = CARTESIAN_POINT ( 'NONE',  ( 40.00000000000000711, -30.00000000000001421, -130.0000000000000000 ) ) ;
#18753 = DIRECTION ( 'NONE',  ( 0.000000000000000000, 0.000000000000000000, -1.000000000000000000 ) ) ;
#18754 =( NAMED_UNIT ( * ) SI_UNIT ( $, .STERADIAN. ) SOLID_ANGLE_UNIT ( ) );
#18755 = CARTESIAN_POINT ( 'NONE',  ( -15.25966316918061949, 10.19618095414378800, 10.05464375018031120 ) ) ;
#18756 = AXIS2_PLACEMENT_3D ( 'NONE', #20379, #5866, #2166 ) ;
#18757 = AXIS2_PLACEMENT_3D ( 'NONE', #9041, #9142, #5851 ) ;
#18758 = CARTESIAN_POINT ( 'NONE',  ( 2.339468227445713921, 3.268109542640642573, 2.447078184617672891E-15 ) ) ;
#18759 = ORIENTED_EDGE ( 'NONE', *, *, #16034, .T. ) ;
#18760 = FACE_OUTER_BOUND ( 'NONE', #16357, .T. ) ;
#18761 = CARTESIAN_POINT ( 'NONE',  ( -1.779019326032424095E-09, -14.79893867758296544, 12.47845808151907754 ) ) ;
#18762 = CARTESIAN_POINT ( 'NONE',  ( 2.500000000000000000, 1.178949249685218525, 2.041999999999999371 ) ) ;
#18763 = AXIS2_PLACEMENT_3D ( 'NONE', #4930, #16269, #16372 ) ;
#18764 = ORIENTED_EDGE ( 'NONE', *, *, #16929, .T. ) ;
#18765 = ADVANCED_FACE ( 'NONE', ( #20887 ), #5315, .T. ) ;
#18766 = CARTESIAN_POINT ( 'NONE',  ( -7.632783294297951215E-14, -4.618802153517020948, -0.3572655899081733644 ) ) ;
#18767 = DIRECTION ( 'NONE',  ( -1.000000000000000000, 0.000000000000000000, 0.000000000000000000 ) ) ;
#18768 = DIRECTION ( 'NONE',  ( 1.000000000000000000, -0.000000000000000000, -0.000000000000000000 ) ) ;
#18769 = ORIENTED_EDGE ( 'NONE', *, *, #11782, .T. ) ;
#18770 = DIRECTION ( 'NONE',  ( 0.000000000000000000, 0.000000000000000000, -1.000000000000000000 ) ) ;
#18771 = ORIENTED_EDGE ( 'NONE', *, *, #3259, .T. ) ;
#18772 = CIRCLE ( 'NONE', #19424, 10.00000000000000178 ) ;
#18773 = DIRECTION ( 'NONE',  ( 0.000000000000000000, 0.000000000000000000, -1.000000000000000000 ) ) ;
#18774 = CARTESIAN_POINT ( 'NONE',  ( 0.000000000000000000, 0.000000000000000000, 43.00000000000000000 ) ) ;
#18775 = ORIENTED_EDGE ( 'NONE', *, *, #7732, .F. ) ;
#18776 = VERTEX_POINT ( 'NONE', #6367 ) ;
#18777 = DIRECTION ( 'NONE',  ( 0.000000000000000000, 0.000000000000000000, -1.000000000000000000 ) ) ;
#18778 = ADVANCED_FACE ( 'NONE', ( #12848, #6771, #1709, #19290, #3485 ), #111, .T. ) ;
#18779 = CARTESIAN_POINT ( 'NONE',  ( 19.99999999999999645, 0.000000000000000000, 0.000000000000000000 ) ) ;
#18780 = FACE_OUTER_BOUND ( 'NONE', #12873, .T. ) ;
#18781 = VECTOR ( 'NONE', #14131, 1000.000000000000000 ) ;
#18782 = CARTESIAN_POINT ( 'NONE',  ( -5.303300858261583706, 5.303300859536630441, -12.58557499981968775 ) ) ;
#18783 = DIRECTION ( 'NONE',  ( -0.000000000000000000, -0.000000000000000000, 1.000000000000000000 ) ) ;
#18784 = CARTESIAN_POINT ( 'NONE',  ( 9.999999999999998224, -44.69367065308685483, 56.44887778834731051 ) ) ;
#18785 = FACE_OUTER_BOUND ( 'NONE', #20420, .T. ) ;
#18786 = ORIENTED_EDGE ( 'NONE', *, *, #20751, .F. ) ;
#18787 = DIRECTION ( 'NONE',  ( 0.000000000000000000, 0.000000000000000000, 1.000000000000000000 ) ) ;
#18788 = ORIENTED_EDGE ( 'NONE', *, *, #6257, .F. ) ;
#18789 = CARTESIAN_POINT ( 'NONE',  ( -2.163827323447878234E-09, -18.00000000000000000, -23.36479999981968803 ) ) ;
#18790 = DIRECTION ( 'NONE',  ( -0.000000000000000000, -0.000000000000000000, -1.000000000000000000 ) ) ;
#18791 = COLOUR_RGB ( '', 0.09019608, 0.27058824, 0.51372549) ;
#18792 = EDGE_LOOP ( 'NONE', ( #3769, #10286 ) ) ;
#18793 = CARTESIAN_POINT ( 'NONE',  ( 19.99999999999999645, -67.51707036274396501, -25.00890260772446894 ) ) ;
#18794 = ORIENTED_EDGE ( 'NONE', *, *, #5630, .F. ) ;
#18795 = CARTESIAN_POINT ( 'NONE',  ( -7.500000000000004441, -1.491842754878798916, -4.633231249912213023 ) ) ;
#18796 = DIRECTION ( 'NONE',  ( 0.000000000000000000, 0.000000000000000000, 1.000000000000000000 ) ) ;
#18797 = CARTESIAN_POINT ( 'NONE',  ( -7.500000000000000888, 1.491842755816075172, -4.044168749912214089 ) ) ;
#18798 = ORIENTED_EDGE ( 'NONE', *, *, #6886, .T. ) ;
#18799 = CARTESIAN_POINT ( 'NONE',  ( 10.00000000000000178, -164.9999999999999716, 73.20000000000000284 ) ) ;
#18800 = EDGE_CURVE ( 'NONE', #14670, #10258, #7346, .T. ) ;
#18801 = EDGE_CURVE ( 'NONE', #1377, #13237, #4981, .T. ) ;
#18802 = CARTESIAN_POINT ( 'NONE',  ( 47.99913302141637672, -4.465704580667244628, 88.98724172780553943 ) ) ;
#18803 = CARTESIAN_POINT ( 'NONE',  ( -17.99999999956958163, 3.580422614997673669, -20.71401874981969371 ) ) ;
#18804 = CARTESIAN_POINT ( 'NONE',  ( 19.99999999999999645, 62.46228066917814203, -18.86519267363391350 ) ) ;
#18805 = DIRECTION ( 'NONE',  ( -1.000000000000000000, 0.000000000000000000, 0.000000000000000000 ) ) ;
#18806 = ADVANCED_FACE ( 'NONE', ( #16421 ), #1909, .T. ) ;
#18807 = ADVANCED_FACE ( 'NONE', ( #2191 ), #13223, .T. ) ;
#18808 = ORIENTED_EDGE ( 'NONE', *, *, #10506, .T. ) ;
#18809 = CARTESIAN_POINT ( 'NONE',  ( -65.00002539999999840, 0.000000000000000000, 0.000000000000000000 ) ) ;
#18810 = DIRECTION ( 'NONE',  ( 0.000000000000000000, 0.000000000000000000, 1.000000000000000000 ) ) ;
#18811 = VERTEX_POINT ( 'NONE', #10072 ) ;
#18812 = CARTESIAN_POINT ( 'NONE',  ( 3.600000000000060485, 10.82531754730546147, 43.00000000000000000 ) ) ;
#18813 = PLANE ( 'NONE',  #12294 ) ;
#18814 = AXIS2_PLACEMENT_3D ( 'NONE', #16045, #6285, #15728 ) ;
#18815 = ORIENTED_EDGE ( 'NONE', *, *, #16850, .T. ) ;
#18816 = CARTESIAN_POINT ( 'NONE',  ( -18.00000000043041126, -3.580422610670022099, -19.39848124981969235 ) ) ;
#18817 = CARTESIAN_POINT ( 'NONE',  ( 0.000000000000000000, 24.01204443665271882, -60.22865198596099390 ) ) ;
#18818 = DIRECTION ( 'NONE',  ( 0.000000000000000000, -0.2697967711570314897, 0.9629172873477973571 ) ) ;
#18819 = EDGE_LOOP ( 'NONE', ( #20760, #9243, #6040, #5825, #4270 ) ) ;
#18820 = EDGE_CURVE ( 'NONE', #17488, #12110, #242, .T. ) ;
#18821 = CARTESIAN_POINT ( 'NONE',  ( 30.00000000000001066, 39.99999999999998579, -120.0000000000000142 ) ) ;
#18822 = EDGE_LOOP ( 'NONE', ( #10817, #14360, #13282 ) ) ;
#18823 = CARTESIAN_POINT ( 'NONE',  ( -62.49999999999999289, -30.00000000000000000, 0.000000000000000000 ) ) ;
#18824 = ORIENTED_EDGE ( 'NONE', *, *, #7528, .F. ) ;
#18825 = EDGE_CURVE ( 'NONE', #19645, #7455, #3795, .T. ) ;
#18826 = VECTOR ( 'NONE', #6629, 1000.000000000000000 ) ;
#18827 = EDGE_CURVE ( 'NONE', #15532, #5814, #1934, .T. ) ;
#18828 = FACE_OUTER_BOUND ( 'NONE', #10038, .T. ) ;
#18829 = AXIS2_PLACEMENT_3D ( 'NONE', #3486, #16127, #16323 ) ;
#18830 = ADVANCED_FACE ( 'NONE', ( #19911 ), #5491, .T. ) ;
#18831 = PRODUCT_DEFINITION_SHAPE ( 'NONE', 'NONE',  #4023 ) ;
#18832 = DIRECTION ( 'NONE',  ( 0.000000000000000000, -1.000000000000000000, 1.287488025362403787E-15 ) ) ;
#18833 = CARTESIAN_POINT ( 'NONE',  ( 2.943691925285398803, -14.79893867793684059, -1.047989331158453830 ) ) ;
#18834 = VERTEX_POINT ( 'NONE', #12080 ) ;
#18835 = FACE_OUTER_BOUND ( 'NONE', #15468, .T. ) ;
#18836 = ORIENTED_EDGE ( 'NONE', *, *, #8071, .F. ) ;
#18837 = CARTESIAN_POINT ( 'NONE',  ( 2.500000000000000000, -1.768423874527823569, 1.021000000000002794 ) ) ;
#18838 = CARTESIAN_POINT ( 'NONE',  ( 16.62983158603121936, 6.888301780572501976, 11.38988750018031126 ) ) ;
#18839 = AXIS2_PLACEMENT_3D ( 'NONE', #126, #13268, #10086 ) ;
#18840 = CARTESIAN_POINT ( 'NONE',  ( 19.99999999999999645, 65.23577793412344761, 1.313498510941937036 ) ) ;
#18841 = CARTESIAN_POINT ( 'NONE',  ( 1.040949779275250179E-14, -85.00000000000000000, 19.00000000000000000 ) ) ;
#18842 = EDGE_CURVE ( 'NONE', #13708, #9945, #8361, .T. ) ;
#18843 = AXIS2_PLACEMENT_3D ( 'NONE', #5136, #13002, #64 ) ;
#18844 = ORIENTED_EDGE ( 'NONE', *, *, #8845, .T. ) ;
#18845 = DIRECTION ( 'NONE',  ( 0.000000000000000000, 0.000000000000000000, -1.000000000000000000 ) ) ;
#18846 = DIRECTION ( 'NONE',  ( -1.000000000000000000, -0.000000000000000000, 0.000000000000000000 ) ) ;
#18847 = ORIENTED_EDGE ( 'NONE', *, *, #11617, .F. ) ;
#18848 = CARTESIAN_POINT ( 'NONE',  ( 20.64343997858507862, -10.14597586228817860, -83.32269133937376182 ) ) ;
#18849 = DIRECTION ( 'NONE',  ( 0.000000000000000000, 0.000000000000000000, -1.000000000000000000 ) ) ;
#18850 = CARTESIAN_POINT ( 'NONE',  ( -3.580422614997674557, -17.99999999956957808, -13.64526874981969407 ) ) ;
#18851 = EDGE_CURVE ( 'NONE', #18161, #14303, #20891, .T. ) ;
#18852 = AXIS2_PLACEMENT_3D ( 'NONE', #666, #13706, #7117 ) ;
#18853 = ORIENTED_EDGE ( 'NONE', *, *, #12228, .F. ) ;
#18854 = DIRECTION ( 'NONE',  ( -1.508455196501572169E-16, 1.000000000000000000, 0.000000000000000000 ) ) ;
#18855 = AXIS2_PLACEMENT_3D ( 'NONE', #20221, #16934, #10584 ) ;
#18856 = CYLINDRICAL_SURFACE ( 'NONE', #15617, 17.50000000000000355 ) ;
#18857 = AXIS2_PLACEMENT_3D ( 'NONE', #101, #8455, #19595 ) ;
#18858 = DIRECTION ( 'NONE',  ( 1.000000000000000000, 0.000000000000000000, 0.000000000000000000 ) ) ;
#18859 = CARTESIAN_POINT ( 'NONE',  ( 30.00000000000000000, -99.99999999999998579, 49.89999999999999858 ) ) ;
#18860 = CARTESIAN_POINT ( 'NONE',  ( 0.000000000000000000, 0.000000000000000000, 0.000000000000000000 ) ) ;
#18861 = CARTESIAN_POINT ( 'NONE',  ( -10.19618095047498230, 15.25966317163203279, 1.218706250180310313 ) ) ;
#18862 = AXIS2_PLACEMENT_3D ( 'NONE', #1149, #15541, #7599 ) ;
#18863 = ADVANCED_FACE ( 'NONE', ( #10277 ), #634, .T. ) ;
#18864 = COLOUR_RGB ( '', 0.40784314, 0.44705882, 0.49803922) ;
#18865 = CARTESIAN_POINT ( 'NONE',  ( 3.673643420401899728, 2.497823135841253706, -0.2484800633749943699 ) ) ;
#18866 = ORIENTED_EDGE ( 'NONE', *, *, #2902, .F. ) ;
#18867 = CARTESIAN_POINT ( 'NONE',  ( 0.000000000000000000, 0.000000000000000000, 126.0000000000000000 ) ) ;
#18868 = CARTESIAN_POINT ( 'NONE',  ( 2.943691928843430450, 14.79893867722910095, 8.060489331519073986 ) ) ;
#18869 = AXIS2_PLACEMENT_3D ( 'NONE', #1064, #9116, #15570 ) ;
#18870 = PLANE ( 'NONE',  #17870 ) ;
#18871 = VERTEX_POINT ( 'NONE', #13782 ) ;
#18872 = CARTESIAN_POINT ( 'NONE',  ( 7.500000000000000000, -9.015933403756343749E-10, 25.48870000018031590 ) ) ;
#18873 = VECTOR ( 'NONE', #74, 1000.000000000000114 ) ;
#18874 = CARTESIAN_POINT ( 'NONE',  ( -12.72792206288791128, -12.72792205982779912, -20.28207499981969164 ) ) ;
#18875 = CARTESIAN_POINT ( 'NONE',  ( 50.00000000000000000, -160.0000000000000000, -79.59486983196737242 ) ) ;
#18876 = ORIENTED_EDGE ( 'NONE', *, *, #20717, .F. ) ;
#18877 = CARTESIAN_POINT ( 'NONE',  ( 30.00000000000000000, -39.99999999999999289, 52.00000000000000000 ) ) ;
#18878 = AXIS2_PLACEMENT_3D ( 'NONE', #1057, #5701, #13668 ) ;
#18879 = ORIENTED_EDGE ( 'NONE', *, *, #4817, .F. ) ;
#18880 = DIRECTION ( 'NONE',  ( 1.000000000000000000, 0.000000000000000000, 0.000000000000000000 ) ) ;
#18881 = CARTESIAN_POINT ( 'NONE',  ( 19.99999999999999645, 0.000000000000000000, 0.000000000000000000 ) ) ;
#18882 = CIRCLE ( 'NONE', #598, 72.00000000007199219 ) ;
#18883 = ORIENTED_EDGE ( 'NONE', *, *, #14170, .T. ) ;
#18884 = ORIENTED_EDGE ( 'NONE', *, *, #16401, .T. ) ;
#18885 = FACE_OUTER_BOUND ( 'NONE', #17927, .T. ) ;
#18886 = CONICAL_SURFACE ( 'NONE', #15783, 4.000000000000000000, 1.047197551196595855 ) ;
#18887 =( NAMED_UNIT ( * ) PLANE_ANGLE_UNIT ( ) SI_UNIT ( $, .RADIAN. ) );
#18888 = DIRECTION ( 'NONE',  ( -0.5000000000000051070, 0.000000000000000000, 0.8660254037844355990 ) ) ;
#18889 = EDGE_CURVE ( 'NONE', #19472, #16235, #18230, .T. ) ;
#18890 = ADVANCED_FACE ( 'NONE', ( #20006 ), #3593, .T. ) ;
#18891 = AXIS2_PLACEMENT_3D ( 'NONE', #19856, #11593, #14987 ) ;
#18892 = CARTESIAN_POINT ( 'NONE',  ( 24.99999999999999645, -99.99999999999998579, 49.89999999999999858 ) ) ;
#18893 = AXIS2_PLACEMENT_3D ( 'NONE', #6642, #10246, #18099 ) ;
#18894 = CARTESIAN_POINT ( 'NONE',  ( 11.17563879758427525, 2.222972768810836719, 18.50035899971319608 ) ) ;
#18895 = DIRECTION ( 'NONE',  ( -1.000000000000000000, 0.000000000000000000, -0.000000000000000000 ) ) ;
#18896 = CARTESIAN_POINT ( 'NONE',  ( 17.50000000000000355, 2.143131898507868643E-15, 43.00000000000000000 ) ) ;
#18897 = LINE ( 'NONE', #14125, #15099 ) ;
#18898 = EDGE_LOOP ( 'NONE', ( #2174, #18505, #11977, #10424 ) ) ;
#18899 = FACE_OUTER_BOUND ( 'NONE', #911, .T. ) ;
#18900 = VERTEX_POINT ( 'NONE', #18327 ) ;
#18901 = CARTESIAN_POINT ( 'NONE',  ( 6.888301780572507305, -16.62983158603121936, -23.95386249981968874 ) ) ;
#18902 = CARTESIAN_POINT ( 'NONE',  ( 40.00000000000000711, -40.00000000000001421, -120.0000000000000142 ) ) ;
#18903 = ORIENTED_EDGE ( 'NONE', *, *, #152, .T. ) ;
#18904 = FACE_OUTER_BOUND ( 'NONE', #5888, .T. ) ;
#18905 = ORIENTED_EDGE ( 'NONE', *, *, #20348, .T. ) ;
#18906 = CARTESIAN_POINT ( 'NONE',  ( 2.500000000000000000, 0.000000000000000000, 0.000000000000000000 ) ) ;
#18907 = DIRECTION ( 'NONE',  ( -0.000000000000000000, -0.000000000000000000, -1.000000000000000000 ) ) ;
#18908 = CARTESIAN_POINT ( 'NONE',  ( 7.500000000000000888, 4.207617034106124418E-15, 0.3738000000023073421 ) ) ;
#18909 = ORIENTED_EDGE ( 'NONE', *, *, #19855, .F. ) ;
#18910 = DIRECTION ( 'NONE',  ( 0.000000000000000000, 0.000000000000000000, 1.000000000000000000 ) ) ;
#18911 = CARTESIAN_POINT ( 'NONE',  ( 19.99999999999999645, -39.37110852956777762, -51.51683813304910586 ) ) ;
#18912 = CARTESIAN_POINT ( 'NONE',  ( -6.888301784570736608, -16.62983158437509346, -22.77573749981969087 ) ) ;
#18913 = CARTESIAN_POINT ( 'NONE',  ( -9.850000000000012079, 0.000000000000000000, 46.00000000000000711 ) ) ;
#18914 = CARTESIAN_POINT ( 'NONE',  ( 2.500000000000000000, 2.357898499370433054, -1.951563910473907981E-15 ) ) ;
#18915 = ORIENTED_EDGE ( 'NONE', *, *, #11179, .T. ) ;
#18916 = DIRECTION ( 'NONE',  ( -1.000000000000000000, 0.000000000000000000, 0.000000000000000000 ) ) ;
#18917 = DIRECTION ( 'NONE',  ( 0.000000000000000000, 0.000000000000000000, 1.000000000000000000 ) ) ;
#18918 = ORIENTED_EDGE ( 'NONE', *, *, #4188, .F. ) ;
#18919 = ADVANCED_FACE ( 'NONE', ( #20232 ), #8678, .F. ) ;
#18920 = CARTESIAN_POINT ( 'NONE',  ( 0.000000000000000000, 15.58726123847851142, 62.93731870009410301 ) ) ;
#18921 = CYLINDRICAL_SURFACE ( 'NONE', #12658, 65.24900000006525147 ) ;
#18922 = EDGE_CURVE ( 'NONE', #4998, #9154, #13794, .T. ) ;
#18923 = ORIENTED_EDGE ( 'NONE', *, *, #12269, .F. ) ;
#18924 = CARTESIAN_POINT ( 'NONE',  ( 3.580422610670020322, -18.00000000043041126, -21.75473124981968809 ) ) ;
#18925 = FACE_OUTER_BOUND ( 'NONE', #11017, .T. ) ;
#18926 = LINE ( 'NONE', #14257, #17745 ) ;
#18927 = ORIENTED_EDGE ( 'NONE', *, *, #18282, .T. ) ;
#18928 = CARTESIAN_POINT ( 'NONE',  ( 19.99999999999999645, 0.000000000000000000, 0.000000000000000000 ) ) ;
#18929 = ORIENTED_EDGE ( 'NONE', *, *, #15226, .T. ) ;
#18930 = CARTESIAN_POINT ( 'NONE',  ( 19.99999999999999645, -56.63599015375694989, 31.56633360682443268 ) ) ;
#18931 = ORIENTED_EDGE ( 'NONE', *, *, #8561, .T. ) ;
#18932 = EDGE_CURVE ( 'NONE', #2970, #8465, #9392, .T. ) ;
#18933 = CARTESIAN_POINT ( 'NONE',  ( 4.000000000000000000, 0.000000000000000000, -5.600000000000000533 ) ) ;
#18934 = DIRECTION ( 'NONE',  ( 0.000000000000000000, -1.000000000000000000, 0.000000000000000000 ) ) ;
#18935 = CARTESIAN_POINT ( 'NONE',  ( -8.382925371439629458, -12.54593441562640876, -9.294864331158457560 ) ) ;
#18936 = VERTEX_POINT ( 'NONE', #734 ) ;
#18937 = DIRECTION ( 'NONE',  ( -1.000000000000000000, 0.000000000000000000, 0.000000000000000000 ) ) ;
#18938 = ORIENTED_EDGE ( 'NONE', *, *, #1555, .T. ) ;
#18939 = CARTESIAN_POINT ( 'NONE',  ( -30.00000000000000000, 40.00000000000000000, -120.0000000000000142 ) ) ;
#18940 = EDGE_CURVE ( 'NONE', #6927, #8003, #13165, .T. ) ;
#18941 = CARTESIAN_POINT ( 'NONE',  ( 6.888301784570727726, 16.62983158437509701, 0.7867625001803102425 ) ) ;
#18942 = EDGE_CURVE ( 'NONE', #10714, #6265, #19877, .T. ) ;
#18943 = DIRECTION ( 'NONE',  ( 1.000000000000000000, 0.000000000000000000, 0.000000000000000000 ) ) ;
#18944 = CARTESIAN_POINT ( 'NONE',  ( 9.999999999999998224, 68.15657073222436679, 23.20952102120305227 ) ) ;
#18945 = EDGE_LOOP ( 'NONE', ( #16107, #18646 ) ) ;
#18946 = ADVANCED_FACE ( 'NONE', ( #2014 ), #16849, .T. ) ;
#18947 = CARTESIAN_POINT ( 'NONE',  ( 19.99999999999999645, 62.46228066917814203, -18.86519267363391350 ) ) ;
#18948 = CARTESIAN_POINT ( 'NONE',  ( 8.900000000000046541, 10.82531754730546147, 43.00000000000000000 ) ) ;
#18949 = VERTEX_POINT ( 'NONE', #8778 ) ;
#18950 = CARTESIAN_POINT ( 'NONE',  ( 11.67222246750216463, -19.83243759501799630, -76.85199795501601727 ) ) ;
#18951 = CARTESIAN_POINT ( 'NONE',  ( -5.303300859536632217, -5.303300858261584594, 3.908175000180308611 ) ) ;
#18952 = CARTESIAN_POINT ( 'NONE',  ( 15.25966316918061239, -10.19618095414378445, -5.987456249819691045 ) ) ;
#18953 = ORIENTED_EDGE ( 'NONE', *, *, #2597, .F. ) ;
#18954 = LINE ( 'NONE', #4640, #11420 ) ;
#18955 = DIRECTION ( 'NONE',  ( 0.000000000000000000, 0.000000000000000000, 1.000000000000000000 ) ) ;
#18956 = DIRECTION ( 'NONE',  ( 0.000000000000000000, 0.000000000000000000, -1.000000000000000000 ) ) ;
#18957 = DIRECTION ( 'NONE',  ( 0.000000000000000000, 0.000000000000000000, -1.000000000000000000 ) ) ;
#18958 = CARTESIAN_POINT ( 'NONE',  ( 39.99999999999964473, -39.99999999999943157, 52.00000000000070344 ) ) ;
#18959 = EDGE_CURVE ( 'NONE', #15567, #9945, #15248, .T. ) ;
#18960 = CARTESIAN_POINT ( 'NONE',  ( -15.25966317163203456, -10.19618095047498230, 8.287456250180309070 ) ) ;
#18961 = ADVANCED_FACE ( 'NONE', ( #20553 ), #3241, .F. ) ;
#18962 = CIRCLE ( 'NONE', #10144, 65.24900000006525147 ) ;
#18963 = CARTESIAN_POINT ( 'NONE',  ( 1.491842756249030622, 7.499999999820669672, -14.27301874981968943 ) ) ;
#18964 = VERTEX_POINT ( 'NONE', #13881 ) ;
#18965 = CARTESIAN_POINT ( 'NONE',  ( 50.00000000000000000, -164.9999999999999716, -90.00000000000001421 ) ) ;
#18966 = CARTESIAN_POINT ( 'NONE',  ( -13.67243654642775041, 5.663308650141531508, 15.42377058151907754 ) ) ;
#18967 = EDGE_CURVE ( 'NONE', #14001, #12159, #15473, .T. ) ;
#18968 = AXIS2_PLACEMENT_3D ( 'NONE', #5216, #5513, #13490 ) ;
#18969 = CARTESIAN_POINT ( 'NONE',  ( 7.500000000000000000, 9.184850993605147944E-16, 126.0000000000000000 ) ) ;
#18970 = ORIENTED_EDGE ( 'NONE', *, *, #12894, .F. ) ;
#18971 = DIRECTION ( 'NONE',  ( 1.000000000000000000, -1.734723475976806848E-16, -0.000000000000000000 ) ) ;
#18972 = CARTESIAN_POINT ( 'NONE',  ( -6.888301780572501976, 16.62983158603122291, -17.33676249981968809 ) ) ;
#18973 = DIRECTION ( 'NONE',  ( -1.000000000000000000, 0.000000000000000000, -0.000000000000000000 ) ) ;
#18974 = ORIENTED_EDGE ( 'NONE', *, *, #17398, .T. ) ;
#18975 = CARTESIAN_POINT ( 'NONE',  ( 5.000000000000000888, 0.000000000000000000, 0.000000000000000000 ) ) ;
#18976 = VERTEX_POINT ( 'NONE', #18969 ) ;
#18977 = CARTESIAN_POINT ( 'NONE',  ( 34.40748350626766694, -26.49925741089600706, -73.93400743789861451 ) ) ;
#18978 = CYLINDRICAL_SURFACE ( 'NONE', #9382, 27.60000000002759535 ) ;
#18979 = AXIS2_PLACEMENT_3D ( 'NONE', #4174, #15514, #6073 ) ;
#18980 = ORIENTED_EDGE ( 'NONE', *, *, #20634, .T. ) ;
#18981 = ORIENTED_EDGE ( 'NONE', *, *, #18023, .F. ) ;
#18982 = LINE ( 'NONE', #4452, #4613 ) ;
#18983 = AXIS2_PLACEMENT_3D ( 'NONE', #8799, #20252, #20353 ) ;
#18984 = CARTESIAN_POINT ( 'NONE',  ( 19.99999999999999645, -6.872116855663586321, 64.47358224882414390 ) ) ;
#18985 = DIRECTION ( 'NONE',  ( -1.000000000000000000, -0.000000000000000000, -0.000000000000000000 ) ) ;
#18986 = CARTESIAN_POINT ( 'NONE',  ( 9.015937996181834148E-10, 7.500000000000000888, -20.83244999981968704 ) ) ;
#18987 = VECTOR ( 'NONE', #1964, 1000.000000000000000 ) ;
#18988 = FACE_OUTER_BOUND ( 'NONE', #20040, .T. ) ;
#18989 = CARTESIAN_POINT ( 'NONE',  ( 18.00000000000000000, 0.000000000000000000, -130.0000000000000000 ) ) ;
#18990 = DIRECTION ( 'NONE',  ( 0.000000000000000000, -0.5000000000000009992, -0.8660254037844380415 ) ) ;
#18991 = VERTEX_POINT ( 'NONE', #4343 ) ;
#18992 = CARTESIAN_POINT ( 'NONE',  ( 2.500000000000000000, -1.178949249685213863, 2.042000000000002924 ) ) ;
#18993 = ORIENTED_EDGE ( 'NONE', *, *, #8798, .T. ) ;
#18994 = CARTESIAN_POINT ( 'NONE',  ( -12.72792205982779912, 12.72792206288790950, -10.40542499981968483 ) ) ;
#18995 = CARTESIAN_POINT ( 'NONE',  ( 30.00000000000000000, 4.299168419249259188, 89.99999999999998579 ) ) ;
#18996 = AXIS2_PLACEMENT_3D ( 'NONE', #15188, #994, #20153 ) ;
#18997 = ORIENTED_EDGE ( 'NONE', *, *, #15200, .T. ) ;
#18998 = DIRECTION ( 'NONE',  ( 0.000000000000000000, 0.000000000000000000, 1.000000000000000000 ) ) ;
#18999 = ORIENTED_EDGE ( 'NONE', *, *, #15288, .T. ) ;
#19000 = CARTESIAN_POINT ( 'NONE',  ( -6.358192988180015881, -4.248408729364577141, -5.222293749819692188 ) ) ;
#19001 = CARTESIAN_POINT ( 'NONE',  ( 0.000000000000000000, -43.56693332842820610, 48.57318520917490190 ) ) ;
#19002 = CARTESIAN_POINT ( 'NONE',  ( 6.929096494179677990, 2.870125741905210859, -0.2152624998196933648 ) ) ;
#19003 = ADVANCED_FACE ( 'NONE', ( #2746 ), #12794, .T. ) ;
#19004 = ORIENTED_EDGE ( 'NONE', *, *, #3690, .F. ) ;
#19005 = DIRECTION ( 'NONE',  ( -1.648349939164583989E-16, 1.000000000000000000, 0.000000000000000000 ) ) ;
#19006 = DIRECTION ( 'NONE',  ( 0.000000000000000000, 0.000000000000000000, 1.000000000000000000 ) ) ;
#19007 = CARTESIAN_POINT ( 'NONE',  ( -10.19618095414378445, -15.25966316918061239, -22.48120624981969229 ) ) ;
#19008 = DIRECTION ( 'NONE',  ( -1.000000000000000000, -0.000000000000000000, -0.000000000000000000 ) ) ;
#19009 = VECTOR ( 'NONE', #7058, 1000.000000000000000 ) ;
#19010 = CARTESIAN_POINT ( 'NONE',  ( 0.000000000000000000, -61.72688495901628869, 19.84591825363989415 ) ) ;
#19011 = AXIS2_PLACEMENT_3D ( 'NONE', #9222, #12731, #12407 ) ;
#19012 = VERTEX_POINT ( 'NONE', #18762 ) ;
#19013 = DIRECTION ( 'NONE',  ( -0.000000000000000000, -0.000000000000000000, 1.000000000000000000 ) ) ;
#19014 = CARTESIAN_POINT ( 'NONE',  ( 19.99999999999999645, 0.000000000000000000, 0.000000000000000000 ) ) ;
#19015 = EDGE_LOOP ( 'NONE', ( #19767, #20679, #4664, #17976 ) ) ;
#19016 = AXIS2_PLACEMENT_3D ( 'NONE', #18632, #8990, #4426 ) ;
#19017 = CARTESIAN_POINT ( 'NONE',  ( 11.50000000000000000, 1.408343819019456176E-15, -68.00000000000000000 ) ) ;
#19018 = DIRECTION ( 'NONE',  ( 0.000000000000000000, 0.2697967711570248284, -0.9629172873477992445 ) ) ;
#19019 = ORIENTED_EDGE ( 'NONE', *, *, #38, .F. ) ;
#19020 = B_SPLINE_CURVE_WITH_KNOTS ( 'NONE', 3,
 ( #4081, #12047, #5779, #18728, #13960, #12255, #12371, #10781, #5678, #10679, #13640, #2622, #12150, #20413, #20088, #19980, #10564, #17028, #17244, #5462, #5567, #2516, #18518, #4409, #9602, #2823, #3135, #19044, #12693, #1355, #7799, #6412, #14274, #15644, #20721, #15862, #1252, #4519, #4831, #7706, #9181, #6209, #16072, #1564, #17460, #9496, #19151, #20621, #12475, #6097, #4728, #9403, #10984, #12575, #4624, #19346 ),
 .UNSPECIFIED., .F., .F.,
 ( 4, 2, 2, 2, 2, 2, 2, 2, 2, 2, 2, 2, 2, 2, 2, 2, 2, 2, 2, 2, 2, 2, 2, 2, 2, 2, 2, 4 ),
 ( 7.372574772901430151E-18, 0.004247431497134123227, 0.008494862994268239514, 0.01061857874283529332, 0.01168043661711882369, 0.01274229449140235233, 0.01698972598853643393, 0.01911344173710348426, 0.02123715748567053460, 0.02336087323423758841, 0.02548458898280463528, 0.02973202047993872901, 0.03185573622850577935, 0.03397945197707283316, 0.03822688347420693383, 0.04035059922277398070, 0.04247431497134102757, 0.04459803071990808832, 0.04565988859419161522, 0.04672174646847514212, 0.05096917796560924280, 0.05203103583989275582, 0.05309289371417626191, 0.05521660946274327408, 0.05734032521131028626, 0.05946404095987729843, 0.06371147245701133666, 0.06795890395414536100 ),
 .UNSPECIFIED. ) ;
#19021 = CARTESIAN_POINT ( 'NONE',  ( 15.25966316918061416, -10.19618095414378622, -4.082856249819688088 ) ) ;
#19022 = CARTESIAN_POINT ( 'NONE',  ( 0.000000000000000000, 36.54710069451126486, -54.05313526368077248 ) ) ;
#19023 = CARTESIAN_POINT ( 'NONE',  ( 52.50000000000000000, -130.0000000000000000, 5.000000000000000000 ) ) ;
#19024 = AXIS2_PLACEMENT_3D ( 'NONE', #4537, #1049, #18956 ) ;
#19025 = ORIENTED_EDGE ( 'NONE', *, *, #3610, .F. ) ;
#19026 = CARTESIAN_POINT ( 'NONE',  ( 0.000000000000000000, 18.50424539729845108, 69.58155576219121485 ) ) ;
#19027 = ORIENTED_EDGE ( 'NONE', *, *, #14431, .F. ) ;
#19028 = CARTESIAN_POINT ( 'NONE',  ( -22.96694501150314238, -24.74873734152930993, -130.0000000000000000 ) ) ;
#19029 = ADVANCED_FACE ( 'NONE', ( #10810 ), #963, .F. ) ;
#19030 = AXIS2_PLACEMENT_3D ( 'NONE', #17704, #19382, #14620 ) ;
#19031 = CIRCLE ( 'NONE', #20020, 2.099999999999997868 ) ;
#19032 = CARTESIAN_POINT ( 'NONE',  ( 4.000000000000004441, -1.549102112939112486, -5.442104661404058241 ) ) ;
#19033 = EDGE_CURVE ( 'NONE', #2254, #6330, #4316, .T. ) ;
#19034 = DIRECTION ( 'NONE',  ( -1.000000000000000000, -0.000000000000000000, -0.000000000000000000 ) ) ;
#19035 = CONTEXT_DEPENDENT_SHAPE_REPRESENTATION ( #1959, #10166 ) ;
#19036 = CARTESIAN_POINT ( 'NONE',  ( -8.382925368423274293, 12.54593441764187745, -6.349551831158453119 ) ) ;
#19037 = CIRCLE ( 'NONE', #75, 27.60000000002759890 ) ;
#19039 = EDGE_LOOP ( 'NONE', ( #13548, #20890, #9329, #19344 ) ) ;
#19038 = AXIS2_PLACEMENT_3D ( 'NONE', #20555, #8894, #12507 ) ;
#19040 = CARTESIAN_POINT ( 'NONE',  ( -7.500000000000004441, 9.706494115430842424E-15, -13.76369999999769256 ) ) ;
#19041 = DIRECTION ( 'NONE',  ( -1.000000000000000000, 0.000000000000000000, 0.000000000000000000 ) ) ;
#19042 = AXIS2_PLACEMENT_3D ( 'NONE', #9646, #6657, #4758 ) ;
#19043 = EDGE_LOOP ( 'NONE', ( #98, #5066, #10224, #4620 ) ) ;
#19044 = CARTESIAN_POINT ( 'NONE',  ( 1.400806052880371855, -21.50201457020015283, 76.03989839961199948 ) ) ;
#19045 = CARTESIAN_POINT ( 'NONE',  ( 3.580422614997667896, 17.99999999956958163, 0.4922312501803097207 ) ) ;
#19046 = DIRECTION ( 'NONE',  ( 0.000000000000000000, 0.3984010898462361228, 0.9172113015054554896 ) ) ;
#19047 = CARTESIAN_POINT ( 'NONE',  ( -10.00000000000000000, 0.000000000000000000, 0.000000000000000000 ) ) ;
#19048 = ORIENTED_EDGE ( 'NONE', *, *, #20190, .T. ) ;
#19049 = DIRECTION ( 'NONE',  ( 1.000000000000000000, 1.836909530733573776E-16, 0.000000000000000000 ) ) ;
#19050 = CARTESIAN_POINT ( 'NONE',  ( -7.459310946700270506E-14, -4.618802153517020948, -5.242734410091827613 ) ) ;
#19051 = ORIENTED_EDGE ( 'NONE', *, *, #17120, .F. ) ;
#19052 = DIRECTION ( 'NONE',  ( -1.000000000000000000, -0.000000000000000000, -0.000000000000000000 ) ) ;
#19053 = AXIS2_PLACEMENT_3D ( 'NONE', #7686, #2809, #20816 ) ;
#19054 = CARTESIAN_POINT ( 'NONE',  ( 5.303300858261583706, -5.303300859536632217, 1.551925000180306213 ) ) ;
#19055 = CARTESIAN_POINT ( 'NONE',  ( -16.62983158437509701, 6.888301784570728614, -10.99448749981968909 ) ) ;
#19056 = CIRCLE ( 'NONE', #7187, 4.250000000000000000 ) ;
#19057 = ORIENTED_EDGE ( 'NONE', *, *, #10028, .F. ) ;
#19058 = DIRECTION ( 'NONE',  ( 0.000000000000000000, 0.3984010898462361228, 0.9172113015054552676 ) ) ;
#19059 = EDGE_CURVE ( 'NONE', #13495, #65, #3618, .T. ) ;
#19060 = CYLINDRICAL_SURFACE ( 'NONE', #16975, 27.60000000002760245 ) ;
#19061 = EDGE_CURVE ( 'NONE', #10075, #10995, #6338, .T. ) ;
#19062 = DIRECTION ( 'NONE',  ( -0.000000000000000000, -0.000000000000000000, 1.000000000000000000 ) ) ;
#19063 = DIRECTION ( 'NONE',  ( 1.000000000000000000, 0.000000000000000000, 0.000000000000000000 ) ) ;
#19064 = DIRECTION ( 'NONE',  ( 1.000000000000000000, 0.000000000000000000, 0.000000000000000000 ) ) ;
#19065 = VECTOR ( 'NONE', #11191, 1000.000000000000000 ) ;
#19066 = CARTESIAN_POINT ( 'NONE',  ( 10.19618095414378978, 15.25966316918061771, 2.985893750180310224 ) ) ;
#19067 = CYLINDRICAL_SURFACE ( 'NONE', #7574, 2.649999999999999467 ) ;
#19068 = ADVANCED_FACE ( 'NONE', ( #17668, #4112, #20448, #10598, #6414 ), #18870, .T. ) ;
#19069 = ORIENTED_EDGE ( 'NONE', *, *, #10275, .F. ) ;
#19070 = CIRCLE ( 'NONE', #5177, 80.00000000000000000 ) ;
#19071 = LINE ( 'NONE', #4547, #13470 ) ;
#19072 = AXIS2_PLACEMENT_3D ( 'NONE', #18681, #11048, #9352 ) ;
#19073 = CARTESIAN_POINT ( 'NONE',  ( 5.663308650141530620, 13.67243654642775041, 17.78002058151907860 ) ) ;
#19074 = DIRECTION ( 'NONE',  ( 0.000000000000000000, -1.000000000000000000, 0.000000000000000000 ) ) ;
#19075 = ORIENTED_EDGE ( 'NONE', *, *, #13385, .F. ) ;
#19076 = DIRECTION ( 'NONE',  ( 1.000000000000000000, 0.000000000000000000, -0.000000000000000000 ) ) ;
#19077 = CARTESIAN_POINT ( 'NONE',  ( 0.000000000000000000, -42.42902769288503606, -49.02903636734241388 ) ) ;
#19078 = DIRECTION ( 'NONE',  ( -1.000000000000000000, 0.000000000000000000, -0.000000000000000000 ) ) ;
#19079 = CIRCLE ( 'NONE', #18727, 10.52399999999999380 ) ;
#19080 = VERTEX_POINT ( 'NONE', #9608 ) ;
#19081 = EDGE_CURVE ( 'NONE', #19301, #13107, #16168, .T. ) ;
#19082 = CARTESIAN_POINT ( 'NONE',  ( 19.99999999999999645, 0.000000000000000000, 0.000000000000000000 ) ) ;
#19083 = ORIENTED_EDGE ( 'NONE', *, *, #18801, .F. ) ;
#19084 = DIRECTION ( 'NONE',  ( 0.000000000000000000, 0.000000000000000000, 1.000000000000000000 ) ) ;
#19085 = DIRECTION ( 'NONE',  ( 0.000000000000000000, -0.5000000000000013323, -0.8660254037844380415 ) ) ;
#19086 = ORIENTED_EDGE ( 'NONE', *, *, #12796, .T. ) ;
#19087 = ORIENTED_EDGE ( 'NONE', *, *, #15835, .T. ) ;
#19088 = CARTESIAN_POINT ( 'NONE',  ( 29.99999999999999645, -106.8586209199411314, -72.71093006432944605 ) ) ;
#19089 = AXIS2_PLACEMENT_3D ( 'NONE', #14044, #11162, #15927 ) ;
#19090 = CIRCLE ( 'NONE', #16710, 27.60000000002759890 ) ;
#19091 = ADVANCED_FACE ( 'NONE', ( #4833 ), #17776, .T. ) ;
#19092 = EDGE_CURVE ( 'NONE', #10684, #6520, #20936, .T. ) ;
#19093 = SURFACE_STYLE_USAGE ( .BOTH. , #7958 ) ;
#19094 = DIRECTION ( 'NONE',  ( -1.000000000000000000, 0.000000000000000000, 0.000000000000000000 ) ) ;
#19095 = EDGE_CURVE ( 'NONE', #15450, #17187, #1670, .T. ) ;
#19096 = DIRECTION ( 'NONE',  ( -0.000000000000000000, -0.000000000000000000, -1.000000000000000000 ) ) ;
#19097 = CARTESIAN_POINT ( 'NONE',  ( -2.222972768810837607, 11.17563879758428769, -5.008171499352571665 ) ) ;
#19098 = CIRCLE ( 'NONE', #9937, 27.60000000002759535 ) ;
#19099 = AXIS2_PLACEMENT_3D ( 'NONE', #16508, #9634, #1987 ) ;
#19100 = CARTESIAN_POINT ( 'NONE',  ( 6.929096493489624642, -2.870125743571141363, -17.88713749981969059 ) ) ;
#19101 = CARTESIAN_POINT ( 'NONE',  ( 19.99999999999999645, 8.857208570070797649, -71.45313048675075152 ) ) ;
#19102 = CARTESIAN_POINT ( 'NONE',  ( 0.000000000000000000, -51.81019761368295207, -38.98425606966110735 ) ) ;
#19103 = DIRECTION ( 'NONE',  ( 0.000000000000000000, 0.000000000000000000, -1.000000000000000000 ) ) ;
#19104 = AXIS2_PLACEMENT_3D ( 'NONE', #3018, #19236, #10859 ) ;
#19105 = VERTEX_POINT ( 'NONE', #5926 ) ;
#19106 = CARTESIAN_POINT ( 'NONE',  ( 2.500000000000000444, 0.000000000000000000, 3.469446951953614189E-15 ) ) ;
#19107 = ORIENTED_EDGE ( 'NONE', *, *, #14150, .T. ) ;
#19108 = CARTESIAN_POINT ( 'NONE',  ( -18.00000000000000000, 2.163826221265758884E-09, -11.58354999981968803 ) ) ;
#19109 = DIRECTION ( 'NONE',  ( -1.000000000000000000, 0.000000000000000000, 0.000000000000000000 ) ) ;
#19110 = VERTEX_POINT ( 'NONE', #14589 ) ;
#19111 = EDGE_CURVE ( 'NONE', #10293, #19589, #63, .T. ) ;
#19112 = DIRECTION ( 'NONE',  ( -0.000000000000000000, 0.000000000000000000, 1.000000000000000000 ) ) ;
#19113 = VERTEX_POINT ( 'NONE', #5811 ) ;
#19114 = CARTESIAN_POINT ( 'NONE',  ( 0.000000000000000000, 0.000000000000000000, 169.0000000000000000 ) ) ;
#19115 = LINE ( 'NONE', #16030, #15829 ) ;
#19116 = DIRECTION ( 'NONE',  ( -1.000000000000000000, 0.000000000000000000, -0.000000000000000000 ) ) ;
#19117 = VECTOR ( 'NONE', #6385, 1000.000000000000000 ) ;
#19118 = ORIENTED_EDGE ( 'NONE', *, *, #15552, .F. ) ;
#19119 = LINE ( 'NONE', #17312, #5591 ) ;
#19120 = CARTESIAN_POINT ( 'NONE',  ( -15.25966317163202923, -10.19618095047497874, -21.89214374981969513 ) ) ;
#19121 = CYLINDRICAL_SURFACE ( 'NONE', #5205, 27.60000000002759890 ) ;
#19122 = CIRCLE ( 'NONE', #6247, 72.00000000007199219 ) ;
#19123 = CARTESIAN_POINT ( 'NONE',  ( -2.870125743571141808, -6.929096493489625530, 12.74411250018030906 ) ) ;
#19124 = ORIENTED_EDGE ( 'NONE', *, *, #16401, .F. ) ;
#19125 = CARTESIAN_POINT ( 'NONE',  ( -1.321505333908964186, 3.855830693249140850, -0.03421028094653189716 ) ) ;
#19126 = EDGE_CURVE ( 'NONE', #1656, #3436, #3949, .T. ) ;
#19127 = CARTESIAN_POINT ( 'NONE',  ( 6.250000000000054179, 10.82531754730546147, 166.0000000000000000 ) ) ;
#19128 = ORIENTED_EDGE ( 'NONE', *, *, #19319, .F. ) ;
#19129 =( GEOMETRIC_REPRESENTATION_CONTEXT ( 3 ) GLOBAL_UNCERTAINTY_ASSIGNED_CONTEXT ( ( #313 ) ) GLOBAL_UNIT_ASSIGNED_CONTEXT ( ( #19598, #4983, #10162 ) ) REPRESENTATION_CONTEXT ( 'NONE', 'WORKASPACE' ) );
#19130 = CARTESIAN_POINT ( 'NONE',  ( -49.35000000000000142, -39.99999999999999289, 5.000000000000000000 ) ) ;
#19131 = DIRECTION ( 'NONE',  ( -0.7071067811865369146, 0.000000000000000000, 0.7071067811865582309 ) ) ;
#19132 = VERTEX_POINT ( 'NONE', #6825 ) ;
#19133 = CARTESIAN_POINT ( 'NONE',  ( -10.19618095414378622, -15.25966316918061416, -20.57660624981969377 ) ) ;
#19134 = CYLINDRICAL_SURFACE ( 'NONE', #11427, 4.000000000000000000 ) ;
#19135 = DIRECTION ( 'NONE',  ( -1.000000000000000000, -0.000000000000000000, -0.000000000000000000 ) ) ;
#19136 = ORIENTED_EDGE ( 'NONE', *, *, #12968, .F. ) ;
#19137 = DIRECTION ( 'NONE',  ( -0.000000000000000000, -0.000000000000000000, -1.000000000000000000 ) ) ;
#19138 = ORIENTED_EDGE ( 'NONE', *, *, #15798, .F. ) ;
#19139 = AXIS2_PLACEMENT_3D ( 'NONE', #8112, #9598, #14386 ) ;
#19140 = LINE ( 'NONE', #15628, #1437 ) ;
#19141 = ORIENTED_EDGE ( 'NONE', *, *, #13374, .T. ) ;
#19142 = AXIS2_PLACEMENT_3D ( 'NONE', #4850, #6636, #3257 ) ;
#19143 = DIRECTION ( 'NONE',  ( -1.000000000000000000, 0.000000000000000000, -0.000000000000000000 ) ) ;
#19144 = CARTESIAN_POINT ( 'NONE',  ( 6.165580000000000283, 0.000000000000000000, 7.567219999999999835 ) ) ;
#19145 = CARTESIAN_POINT ( 'NONE',  ( -10.46442989454075878, -10.46442989202484242, -18.42533308115845969 ) ) ;
#19146 = ORIENTED_EDGE ( 'NONE', *, *, #19438, .T. ) ;
#19147 = CARTESIAN_POINT ( 'NONE',  ( 4.248408729364576253, -6.358192988180015881, -17.00354374981969130 ) ) ;
#19148 = ADVANCED_FACE ( 'NONE', ( #10019 ), #8631, .T. ) ;
#19149 = DIRECTION ( 'NONE',  ( -1.000000000000000000, -0.000000000000000000, -0.000000000000000000 ) ) ;
#19150 = ORIENTED_EDGE ( 'NONE', *, *, #12460, .F. ) ;
#19151 = CARTESIAN_POINT ( 'NONE',  ( 17.18811727938071598, -12.93019132815889627, 81.11311984140925802 ) ) ;
#19152 = CARTESIAN_POINT ( 'NONE',  ( -31.75000000000000000, 10.52399999999999380, 0.000000000000000000 ) ) ;
#19153 = CARTESIAN_POINT ( 'NONE',  ( -65.00002539999999840, 0.000000000000000000, 0.000000000000000000 ) ) ;
#19154 = EDGE_LOOP ( 'NONE', ( #20810, #11426, #2158, #6783 ) ) ;
#19155 = VECTOR ( 'NONE', #9048, 1000.000000000000000 ) ;
#19156 = LINE ( 'NONE', #19459, #6337 ) ;
#19157 = DIRECTION ( 'NONE',  ( -1.000000000000000000, 0.000000000000000000, 0.000000000000000000 ) ) ;
#19158 = ORIENTED_EDGE ( 'NONE', *, *, #11143, .F. ) ;
#19159 = CARTESIAN_POINT ( 'NONE',  ( -20.49352359574021065, -10.45859730899524820, -83.05345869059719632 ) ) ;
#19160 = AXIS2_PLACEMENT_3D ( 'NONE', #12527, #4464, #19103 ) ;
#19161 = CARTESIAN_POINT ( 'NONE',  ( -10.19618095414378445, -15.25966316918061239, -22.48120624981969584 ) ) ;
#19162 = ORIENTED_EDGE ( 'NONE', *, *, #20769, .T. ) ;
#19163 = DIRECTION ( 'NONE',  ( 0.000000000000000000, 0.5195839500354288987, 0.8544194045464914566 ) ) ;
#19164 = CYLINDRICAL_SURFACE ( 'NONE', #1117, 27.60000000002759535 ) ;
#19165 = CARTESIAN_POINT ( 'NONE',  ( -12.50000000000000711, 1.734723475976807094E-13, 51.00000000000001421 ) ) ;
#19166 = CARTESIAN_POINT ( 'NONE',  ( 16.62983158437509701, -6.888301784570740161, 14.47261250018030942 ) ) ;
#19167 = AXIS2_PLACEMENT_3D ( 'NONE', #6582, #24, #9972 ) ;
#19168 = CARTESIAN_POINT ( 'NONE',  ( 7.500000000179346316, 1.491842754445843244, -12.50583124981968908 ) ) ;
#19169 = EDGE_LOOP ( 'NONE', ( #20144, #3376, #4718, #6267, #17540 ) ) ;
#19170 = DIRECTION ( 'NONE',  ( -1.000000000000000000, 0.000000000000000000, -0.000000000000000000 ) ) ;
#19171 = CIRCLE ( 'NONE', #5955, 2.649999999999987477 ) ;
#19172 = VECTOR ( 'NONE', #6725, 1000.000000000000000 ) ;
#19173 = CARTESIAN_POINT ( 'NONE',  ( 14.79893867758296544, -1.779016607511491977E-09, 10.12220808151907470 ) ) ;
#19174 = DIRECTION ( 'NONE',  ( 0.000000000000000000, 0.000000000000000000, 1.000000000000000000 ) ) ;
#19175 = EDGE_CURVE ( 'NONE', #18021, #8383, #18882, .T. ) ;
#19176 = ORIENTED_EDGE ( 'NONE', *, *, #20743, .T. ) ;
#19177 = DIRECTION ( 'NONE',  ( -1.000000000000000000, 0.000000000000000000, -0.000000000000000000 ) ) ;
#19178 = EDGE_CURVE ( 'NONE', #15776, #16643, #18152, .T. ) ;
#19179 = CIRCLE ( 'NONE', #12062, 27.60000000002760245 ) ;
#19180 = CARTESIAN_POINT ( 'NONE',  ( 30.00000000000000000, -85.00000000000000000, -1.040949779275250179E-14 ) ) ;
#19181 = DIRECTION ( 'NONE',  ( -1.000000000000000000, 1.734723475976806848E-16, 0.000000000000000000 ) ) ;
#19182 = EDGE_LOOP ( 'NONE', ( #6021, #17890 ) ) ;
#19183 = CARTESIAN_POINT ( 'NONE',  ( 17.50000000000000355, 2.143131898507868643E-15, 43.00000000000000000 ) ) ;
#19184 = AXIS2_PLACEMENT_3D ( 'NONE', #4878, #11536, #13148 ) ;
#19185 = VERTEX_POINT ( 'NONE', #370 ) ;
#19186 = DIRECTION ( 'NONE',  ( -1.000000000000000000, 0.000000000000000000, 0.000000000000000000 ) ) ;
#19187 = DIRECTION ( 'NONE',  ( 1.000000000000000000, 0.000000000000000000, 0.000000000000000000 ) ) ;
#19188 = AXIS2_PLACEMENT_3D ( 'NONE', #9947, #202, #11642 ) ;
#19189 = EDGE_LOOP ( 'NONE', ( #12707, #18005, #7601 ) ) ;
#19190 = EDGE_CURVE ( 'NONE', #44, #10605, #6627, .T. ) ;
#19191 = EDGE_LOOP ( 'NONE', ( #1151, #5933, #7754, #2928 ) ) ;
#19192 = DIRECTION ( 'NONE',  ( 0.000000000000000000, 0.000000000000000000, 1.000000000000000000 ) ) ;
#19193 = AXIS2_PLACEMENT_3D ( 'NONE', #17383, #1288, #9115 ) ;
#19194 = CARTESIAN_POINT ( 'NONE',  ( 0.000000000000000000, 70.68211945903188109, 13.71269443944231980 ) ) ;
#19195 = CARTESIAN_POINT ( 'NONE',  ( 0.000000000000000000, 0.000000000000000000, 43.00000000000000000 ) ) ;
#19196 = CARTESIAN_POINT ( 'NONE',  ( -7.902369976724401113, 7.902369978624329327, -15.31676524935257078 ) ) ;
#19197 = EDGE_CURVE ( 'NONE', #1468, #19897, #8705, .T. ) ;
#19198 = CARTESIAN_POINT ( 'NONE',  ( 11.17563879731704723, -1.343450868547281106E-09, 18.79489024971320177 ) ) ;
#19199 = AXIS2_PLACEMENT_3D ( 'NONE', #6221, #20637, #19163 ) ;
#19200 = CARTESIAN_POINT ( 'NONE',  ( -2.500000000000002220, 0.000000000000000000, -5.574599999999999334 ) ) ;
#19201 = DIRECTION ( 'NONE',  ( -0.000000000000000000, -0.000000000000000000, 1.000000000000000000 ) ) ;
#19202 = CARTESIAN_POINT ( 'NONE',  ( 6.249999999999902300, -10.82531754730554496, -40.00000000000000000 ) ) ;
#19203 = EDGE_CURVE ( 'NONE', #15210, #5576, #2177, .T. ) ;
#19204 = VECTOR ( 'NONE', #20939, 1000.000000000000000 ) ;
#19205 = ORIENTED_EDGE ( 'NONE', *, *, #3654, .F. ) ;
#19206 = PLANE ( 'NONE',  #16650 ) ;
#19207 = EDGE_CURVE ( 'NONE', #16643, #15842, #18186, .T. ) ;
#19208 = VERTEX_POINT ( 'NONE', #17881 ) ;
#19209 = CARTESIAN_POINT ( 'NONE',  ( -10.19618095047498052, 15.25966317163203101, -19.53589374981968518 ) ) ;
#19210 = DIRECTION ( 'NONE',  ( 1.000000000000000000, 0.000000000000000000, 0.000000000000000000 ) ) ;
#19211 = VERTEX_POINT ( 'NONE', #13311 ) ;
#19212 = DIRECTION ( 'NONE',  ( 0.000000000000000000, 0.000000000000000000, 1.000000000000000000 ) ) ;
#19213 = ORIENTED_EDGE ( 'NONE', *, *, #17398, .F. ) ;
#19214 = DIRECTION ( 'NONE',  ( 0.000000000000000000, 0.000000000000000000, -1.000000000000000000 ) ) ;
#19215 = CARTESIAN_POINT ( 'NONE',  ( -7.500000000000004441, 9.706494107352906755E-15, -4.338699999997692736 ) ) ;
#19216 = EDGE_CURVE ( 'NONE', #5326, #6733, #16452, .T. ) ;
#19217 = ORIENTED_EDGE ( 'NONE', *, *, #7803, .F. ) ;
#19218 = CARTESIAN_POINT ( 'NONE',  ( 19.99999999999999645, -3.141410481201533322, 65.17333458706184501 ) ) ;
#19219 = CIRCLE ( 'NONE', #6019, 80.00000000000000000 ) ;
#19220 = CARTESIAN_POINT ( 'NONE',  ( 0.000000000000000000, 0.000000000000000000, -5.600000000000000533 ) ) ;
#19221 = DIRECTION ( 'NONE',  ( 1.000000000000000000, 0.000000000000000000, 0.000000000000000000 ) ) ;
#19222 = CIRCLE ( 'NONE', #11765, 2.500000000000000888 ) ;
#19223 = CARTESIAN_POINT ( 'NONE',  ( 40.00000000000000711, -40.00000000000001421, -130.0000000000000000 ) ) ;
#19224 = EDGE_CURVE ( 'NONE', #5705, #13762, #5348, .T. ) ;
#19225 = ORIENTED_EDGE ( 'NONE', *, *, #803, .F. ) ;
#19226 = EDGE_CURVE ( 'NONE', #3060, #5677, #13751, .T. ) ;
#19227 = DIRECTION ( 'NONE',  ( -1.000000000000000000, 0.000000000000000000, 0.000000000000000000 ) ) ;
#19228 = DIRECTION ( 'NONE',  ( 0.000000000000000000, 0.000000000000000000, 1.000000000000000000 ) ) ;
#19229 = ORIENTED_EDGE ( 'NONE', *, *, #14716, .F. ) ;
#19230 = CARTESIAN_POINT ( 'NONE',  ( 19.99999999999999645, -62.46228066917801414, 18.86519267363435048 ) ) ;
#19231 = DIRECTION ( 'NONE',  ( 0.000000000000000000, 0.000000000000000000, 1.000000000000000000 ) ) ;
#19232 = ORIENTED_EDGE ( 'NONE', *, *, #2610, .T. ) ;
#19233 = CYLINDRICAL_SURFACE ( 'NONE', #8163, 2.649999999999999467 ) ;
#19234 = EDGE_CURVE ( 'NONE', #5499, #9196, #10356, .T. ) ;
#19235 = DIRECTION ( 'NONE',  ( -1.000000000000000000, 0.000000000000000000, 0.000000000000000000 ) ) ;
#19236 = DIRECTION ( 'NONE',  ( 0.000000000000000000, -1.000000000000000000, 0.000000000000000000 ) ) ;
#19237 = ORIENTED_EDGE ( 'NONE', *, *, #3492, .F. ) ;
#19238 = DIRECTION ( 'NONE',  ( -1.000000000000000000, 0.000000000000000000, 0.000000000000000000 ) ) ;
#19239 = ORIENTED_EDGE ( 'NONE', *, *, #11818, .T. ) ;
#19240 = DIRECTION ( 'NONE',  ( -1.000000000000000000, -0.000000000000000000, -0.000000000000000000 ) ) ;
#19241 = ORIENTED_EDGE ( 'NONE', *, *, #5461, .F. ) ;
#19242 = DIRECTION ( 'NONE',  ( -0.000000000000000000, -0.000000000000000000, -1.000000000000000000 ) ) ;
#19243 = CARTESIAN_POINT ( 'NONE',  ( 6.249999999999902300, -10.82531754730554496, -43.00000000000000000 ) ) ;
#19244 = CARTESIAN_POINT ( 'NONE',  ( 2.943691928843431782, 14.79893867722910628, -14.59642683115845863 ) ) ;
#19245 = ORIENTED_EDGE ( 'NONE', *, *, #5186, .T. ) ;
#19246 = LINE ( 'NONE', #1664, #18109 ) ;
#19247 = DIRECTION ( 'NONE',  ( -1.000000000000000000, -0.000000000000000000, -0.000000000000000000 ) ) ;
#19248 = ORIENTED_EDGE ( 'NONE', *, *, #4734, .T. ) ;
#19249 = DIRECTION ( 'NONE',  ( 0.000000000000000000, 1.000000000000000000, -1.471414886128461471E-15 ) ) ;
#19250 = DIRECTION ( 'NONE',  ( 0.000000000000000000, -1.000000000000000000, 1.287488025362403787E-15 ) ) ;
#19251 = FACE_OUTER_BOUND ( 'NONE', #9492, .T. ) ;
#19252 = EDGE_LOOP ( 'NONE', ( #11072, #5426 ) ) ;
#19253 = CARTESIAN_POINT ( 'NONE',  ( -4.000000000000000000, 0.000000000000000000, 0.000000000000000000 ) ) ;
#19254 = CARTESIAN_POINT ( 'NONE',  ( 0.000000000000000000, 0.000000000000000000, 0.000000000000000000 ) ) ;
#19255 = AXIS2_PLACEMENT_3D ( 'NONE', #4575, #9132, #17515 ) ;
#19256 = ORIENTED_EDGE ( 'NONE', *, *, #19226, .T. ) ;
#19257 = CARTESIAN_POINT ( 'NONE',  ( -17.19777750590179366, -15.33753975069672748, -79.43571204742693226 ) ) ;
#19258 = CARTESIAN_POINT ( 'NONE',  ( 0.000000000000000000, 2.357898499370431722, -2.818925648462311528E-15 ) ) ;
#19259 = DIRECTION ( 'NONE',  ( -0.000000000000000000, -0.000000000000000000, 1.000000000000000000 ) ) ;
#19260 = EDGE_CURVE ( 'NONE', #10658, #1607, #8652, .T. ) ;
#19261 = EDGE_LOOP ( 'NONE', ( #6803, #465 ) ) ;
#19262 = CARTESIAN_POINT ( 'NONE',  ( 9.470358143689558972, -1.138454911109687490E-09, -38.52172829718890057 ) ) ;
#19263 =( NAMED_UNIT ( * ) SI_UNIT ( $, .STERADIAN. ) SOLID_ANGLE_UNIT ( ) );
#19264 = CARTESIAN_POINT ( 'NONE',  ( -30.00000000000000000, -85.00000000000000000, 8.999999999999984013 ) ) ;
#19265 = DIRECTION ( 'NONE',  ( 6.982962677686266711E-15, 0.000000000000000000, -1.000000000000000000 ) ) ;
#19266 = CARTESIAN_POINT ( 'NONE',  ( -16.62983158603122646, -6.888301780572501976, -10.26801249981969200 ) ) ;
#19267 = DIRECTION ( 'NONE',  ( 0.000000000000000000, -1.000000000000000000, 0.000000000000000000 ) ) ;
#19268 = DIRECTION ( 'NONE',  ( -1.000000000000000000, 0.000000000000000000, 0.000000000000000000 ) ) ;
#19269 = CARTESIAN_POINT ( 'NONE',  ( 12.54593441764186679, 8.382925368423272516, -9.611385668480929567 ) ) ;
#19270 = DIRECTION ( 'NONE',  ( 1.000000000000000000, 0.000000000000000000, 0.000000000000000000 ) ) ;
#19271 = ORIENTED_EDGE ( 'NONE', *, *, #5565, .F. ) ;
#19272 = DIRECTION ( 'NONE',  ( -1.000000000000000000, -0.000000000000000000, -0.000000000000000000 ) ) ;
#19273 = CARTESIAN_POINT ( 'NONE',  ( 2.870125743571140475, 6.929096493489632635, 23.72151250018031732 ) ) ;
#19274 = CARTESIAN_POINT ( 'NONE',  ( 50.00000000000000000, -164.9999999999999716, -75.59990929030051632 ) ) ;
#19275 = ORIENTED_EDGE ( 'NONE', *, *, #6854, .T. ) ;
#19276 = DIRECTION ( 'NONE',  ( -1.000000000000000000, 0.000000000000000000, 0.000000000000000000 ) ) ;
#19277 = ORIENTED_EDGE ( 'NONE', *, *, #6020, .F. ) ;
#19278 = CYLINDRICAL_SURFACE ( 'NONE', #4102, 27.60000000002759890 ) ;
#19279 = DIRECTION ( 'NONE',  ( 0.000000000000000000, 0.000000000000000000, -1.000000000000000000 ) ) ;
#19280 = ADVANCED_FACE ( 'NONE', ( #16578 ), #3546, .T. ) ;
#19281 = EDGE_LOOP ( 'NONE', ( #6960, #13424, #8831, #12361 ) ) ;
#19282 = ORIENTED_EDGE ( 'NONE', *, *, #6484, .F. ) ;
#19283 = LINE ( 'NONE', #11025, #220 ) ;
#19284 = VECTOR ( 'NONE', #19249, 1000.000000000000000 ) ;
#19285 = DIRECTION ( 'NONE',  ( -1.000000000000000000, 0.000000000000000000, 0.000000000000000000 ) ) ;
#19286 = EDGE_CURVE ( 'NONE', #5950, #8014, #11380, .T. ) ;
#19287 = CARTESIAN_POINT ( 'NONE',  ( 11.17563879731705789, -1.343450868547281933E-09, -2.357390249352570688 ) ) ;
#19288 = CARTESIAN_POINT ( 'NONE',  ( -7.902369978624323110, -7.902369976724391343, 3.479265249713199282 ) ) ;
#19289 = DIRECTION ( 'NONE',  ( 1.000000000000000000, -0.000000000000000000, -0.000000000000000000 ) ) ;
#19290 = FACE_BOUND ( 'NONE', #3440, .T. ) ;
#19291 = CARTESIAN_POINT ( 'NONE',  ( 19.99999999999999645, 31.98952867950403345, -56.39803944231551469 ) ) ;
#19292 = ADVANCED_FACE ( 'NONE', ( #8216 ), #3745, .F. ) ;
#19293 = ORIENTED_EDGE ( 'NONE', *, *, #11538, .T. ) ;
#19294 = LINE ( 'NONE', #8375, #12611 ) ;
#19295 = ORIENTED_EDGE ( 'NONE', *, *, #20901, .F. ) ;
#19296 = AXIS2_PLACEMENT_3D ( 'NONE', #3817, #16761, #14760 ) ;
#19297 = CARTESIAN_POINT ( 'NONE',  ( 18.00000000000000000, -2.163824016901520184E-09, 13.88355000018031404 ) ) ;
#19298 = DIRECTION ( 'NONE',  ( -1.000000000000000000, 0.000000000000000000, -0.000000000000000000 ) ) ;
#19299 = EDGE_LOOP ( 'NONE', ( #14321, #5091 ) ) ;
#19300 = CARTESIAN_POINT ( 'NONE',  ( 0.000000000000000000, -60.35829202194891252, 24.78524934717529504 ) ) ;
#19301 = VERTEX_POINT ( 'NONE', #16687 ) ;
#19302 = DIRECTION ( 'NONE',  ( -0.000000000000000000, 0.000000000000000000, 1.000000000000000000 ) ) ;
#19303 = CARTESIAN_POINT ( 'NONE',  ( 30.47229197614141682, -42.00316239176417099, 71.34654888422416263 ) ) ;
#19304 = ORIENTED_EDGE ( 'NONE', *, *, #7144, .T. ) ;
#19305 = VECTOR ( 'NONE', #2962, 1000.000000000000000 ) ;
#19306 = EDGE_LOOP ( 'NONE', ( #14729, #11202, #9387, #14286 ) ) ;
#19307 = DIRECTION ( 'NONE',  ( -1.000000000000000000, 0.000000000000000000, 0.000000000000000000 ) ) ;
#19308 = CYLINDRICAL_SURFACE ( 'NONE', #14308, 2.650000000000000355 ) ;
#19309 = CARTESIAN_POINT ( 'NONE',  ( 4.000000000000003553, 1.557668341133516154, -0.1596965656957575475 ) ) ;
#19310 = EDGE_CURVE ( 'NONE', #19185, #2818, #4994, .T. ) ;
#19311 = EDGE_CURVE ( 'NONE', #440, #3863, #14693, .T. ) ;
#19312 = AXIS2_PLACEMENT_3D ( 'NONE', #10119, #13415, #13721 ) ;
#19313 = CARTESIAN_POINT ( 'NONE',  ( 19.99999999999999645, 0.000000000000000000, 0.000000000000000000 ) ) ;
#19314 = EDGE_LOOP ( 'NONE', ( #13301, #6937, #18769, #8164, #621, #7737, #15409, #10911, #793 ) ) ;
#19315 = DIRECTION ( 'NONE',  ( -1.000000000000000000, 0.000000000000000000, 0.000000000000000000 ) ) ;
#19316 = EDGE_CURVE ( 'NONE', #8735, #10739, #7313, .T. ) ;
#19317 = CARTESIAN_POINT ( 'NONE',  ( -7.500000000000004441, 9.706494115430842424E-15, -13.76369999999769256 ) ) ;
#19318 = AXIS2_PLACEMENT_3D ( 'NONE', #11695, #12983, #147 ) ;
#19319 = EDGE_CURVE ( 'NONE', #16258, #764, #14096, .T. ) ;
#19320 = DIRECTION ( 'NONE',  ( 1.000000000000000000, -0.000000000000000000, 0.000000000000000000 ) ) ;
#19321 = DIRECTION ( 'NONE',  ( 0.000000000000000000, 0.000000000000000000, 1.000000000000000000 ) ) ;
#19322 = VERTEX_POINT ( 'NONE', #5441 ) ;
#19323 = DIRECTION ( 'NONE',  ( -1.000000000000000000, 0.000000000000000000, 0.000000000000000000 ) ) ;
#19324 = CARTESIAN_POINT ( 'NONE',  ( -10.00000000000000000, 0.000000000000000000, 0.000000000000000000 ) ) ;
#19325 = DIRECTION ( 'NONE',  ( -0.000000000000000000, -0.000000000000000000, 1.000000000000000000 ) ) ;
#19326 = VERTEX_POINT ( 'NONE', #12026 ) ;
#19327 = CARTESIAN_POINT ( 'NONE',  ( 8.900000000000046541, 10.82531754730546147, 129.0000000000000000 ) ) ;
#19328 = EDGE_LOOP ( 'NONE', ( #8278, #12342 ) ) ;
#19329 = CARTESIAN_POINT ( 'NONE',  ( 2.500000000000000000, 2.357898499370431722, -2.818925648462311528E-15 ) ) ;
#19330 = EDGE_CURVE ( 'NONE', #7692, #16592, #19171, .T. ) ;
#19331 = ORIENTED_EDGE ( 'NONE', *, *, #20717, .T. ) ;
#19332 = EDGE_CURVE ( 'NONE', #3628, #16612, #20280, .T. ) ;
#19333 = AXIS2_PLACEMENT_3D ( 'NONE', #9607, #16272, #16074 ) ;
#19334 = VECTOR ( 'NONE', #9014, 1000.000000000000000 ) ;
#19335 = CARTESIAN_POINT ( 'NONE',  ( 19.99999999999999645, 0.000000000000000000, 0.000000000000000000 ) ) ;
#19336 = ADVANCED_FACE ( 'NONE', ( #17117 ), #2603, .T. ) ;
#19337 = CARTESIAN_POINT ( 'NONE',  ( 19.99999999999999645, 60.35829202194909016, -24.78524934717487227 ) ) ;
#19338 = CIRCLE ( 'NONE', #14610, 2.649999999999994582 ) ;
#19339 = CARTESIAN_POINT ( 'NONE',  ( 1.343451552857795926E-09, 11.17563879731705789, 23.56135975064743349 ) ) ;
#19340 = ORIENTED_EDGE ( 'NONE', *, *, #6120, .T. ) ;
#19342 = EDGE_CURVE ( 'NONE', #8829, #10337, #20166, .T. ) ;
#19341 = CARTESIAN_POINT ( 'NONE',  ( 19.99999999999999645, -39.37110852956848817, 51.51683813304857296 ) ) ;
#19343 = CARTESIAN_POINT ( 'NONE',  ( 19.99999999999999645, -42.42902769288568976, 49.02903636734183124 ) ) ;
#19344 = ORIENTED_EDGE ( 'NONE', *, *, #16642, .T. ) ;
#19345 = AXIS2_PLACEMENT_3D ( 'NONE', #12842, #14536, #19392 ) ;
#19346 = CARTESIAN_POINT ( 'NONE',  ( 21.18805271706017024, -3.649167310370820871, 90.00000000000000000 ) ) ;
#19347 = AXIS2_PLACEMENT_3D ( 'NONE', #10934, #5842, #15811 ) ;
#19348 = FACE_OUTER_BOUND ( 'NONE', #11311, .T. ) ;
#19349 = AXIS2_PLACEMENT_3D ( 'NONE', #13862, #10887, #20309 ) ;
#19350 = DIRECTION ( 'NONE',  ( 1.000000000000000000, 0.000000000000000000, 0.000000000000000000 ) ) ;
#19351 = DIRECTION ( 'NONE',  ( -1.000000000000000000, -0.000000000000000000, -0.000000000000000000 ) ) ;
#19352 = ORIENTED_EDGE ( 'NONE', *, *, #18287, .F. ) ;
#19353 = FACE_BOUND ( 'NONE', #14180, .T. ) ;
#19354 = AXIS2_PLACEMENT_3D ( 'NONE', #6923, #6224, #12710 ) ;
#19355 = ORIENTED_EDGE ( 'NONE', *, *, #17127, .T. ) ;
#19356 = CARTESIAN_POINT ( 'NONE',  ( 0.000000000000000000, 0.000000000000000000, -25.03750572909317285 ) ) ;
#19357 = ADVANCED_FACE ( 'NONE', ( #15309 ), #15206, .T. ) ;
#19358 = CARTESIAN_POINT ( 'NONE',  ( 30.00000000000000000, -42.57363661491096707, -66.38288848018790134 ) ) ;
#19359 = CARTESIAN_POINT ( 'NONE',  ( 7.500000000000009770, -8.788009017158368372E-15, -2.786299999997682519 ) ) ;
#19360 = ORIENTED_EDGE ( 'NONE', *, *, #7843, .F. ) ;
#19361 = CYLINDRICAL_SURFACE ( 'NONE', #10388, 27.60000000002759890 ) ;
#19362 = AXIS2_PLACEMENT_3D ( 'NONE', #2223, #14846, #8682 ) ;
#19363 = PLANE ( 'NONE',  #14630 ) ;
#19364 = SHAPE_DEFINITION_REPRESENTATION ( #5258, #8160 ) ;
#19365 = CARTESIAN_POINT ( 'NONE',  ( -18.00000000000000355, 2.163826221265759298E-09, -19.10394999981969377 ) ) ;
#19366 = VERTEX_POINT ( 'NONE', #5661 ) ;
#19367 = FACE_BOUND ( 'NONE', #15896, .T. ) ;
#19368 = DIRECTION ( 'NONE',  ( 0.000000000000000000, -1.000000000000000000, 0.000000000000000000 ) ) ;
#19369 = CARTESIAN_POINT ( 'NONE',  ( -5.663308646854335215, 13.67243654778934925, -11.67310441848092673 ) ) ;
#19370 = EDGE_CURVE ( 'NONE', #8470, #1628, #18486, .T. ) ;
#19371 = CARTESIAN_POINT ( 'NONE',  ( 23.13963350654227824, -26.35784117651622793, -120.0000000000000142 ) ) ;
#19372 = VECTOR ( 'NONE', #1163, 1000.000000000000000 ) ;
#19373 = AXIS2_PLACEMENT_3D ( 'NONE', #7138, #19584, #3464 ) ;
#19374 = ORIENTED_EDGE ( 'NONE', *, *, #18438, .T. ) ;
#19375 = CYLINDRICAL_SURFACE ( 'NONE', #17018, 27.60000000002760245 ) ;
#19376 = LINE ( 'NONE', #8349, #8342 ) ;
#19377 = CARTESIAN_POINT ( 'NONE',  ( 38.21638006031223966, -18.69091178866597147, 71.83091255860625779 ) ) ;
#19378 = AXIS2_PLACEMENT_3D ( 'NONE', #3678, #10363, #8449 ) ;
#19379 = VERTEX_POINT ( 'NONE', #2281 ) ;
#19380 = CARTESIAN_POINT ( 'NONE',  ( 19.99999999999999645, 5.762283366691162811, 64.99406197038673838 ) ) ;
#19381 = ORIENTED_EDGE ( 'NONE', *, *, #17387, .T. ) ;
#19382 = DIRECTION ( 'NONE',  ( -0.000000000000000000, -1.000000000000000000, -0.000000000000000000 ) ) ;
#19383 = CARTESIAN_POINT ( 'NONE',  ( 18.00000000043040771, 3.580422610670018546, 21.10941875018031055 ) ) ;
#19384 = VERTEX_POINT ( 'NONE', #8739 ) ;
#19385 = AXIS2_PLACEMENT_3D ( 'NONE', #16594, #2398, #10140 ) ;
#19386 = ORIENTED_EDGE ( 'NONE', *, *, #19438, .F. ) ;
#19387 = DIRECTION ( 'NONE',  ( -1.000000000000000000, 0.000000000000000000, -0.000000000000000000 ) ) ;
#19388 = DIRECTION ( 'NONE',  ( 0.000000000000000000, 0.000000000000000000, 1.000000000000000000 ) ) ;
#19389 = LINE ( 'NONE', #3586, #2159 ) ;
#19390 = AXIS2_PLACEMENT_3D ( 'NONE', #8850, #10776, #12143 ) ;
#19391 = AXIS2_PLACEMENT_3D ( 'NONE', #17697, #6438, #4660 ) ;
#19392 = DIRECTION ( 'NONE',  ( -1.000000000000000000, 0.000000000000000000, 0.000000000000000000 ) ) ;
#19393 = CARTESIAN_POINT ( 'NONE',  ( 1.491842756249030622, 7.499999999820669672, 23.42698125018031519 ) ) ;
#19394 = CARTESIAN_POINT ( 'NONE',  ( 4.276731812588566939, -10.32494394809438809, 11.13707774971319964 ) ) ;
#19395 = EDGE_CURVE ( 'NONE', #13475, #16876, #15830, .T. ) ;
#19396 = DIRECTION ( 'NONE',  ( 0.000000000000000000, 0.000000000000000000, -1.000000000000000000 ) ) ;
#19397 = VECTOR ( 'NONE', #20336, 1000.000000000000000 ) ;
#19398 = CARTESIAN_POINT ( 'NONE',  ( -6.177131623262581250, 0.000000000000000000, 0.000000000000000000 ) ) ;
#19399 = DIRECTION ( 'NONE',  ( -1.000000000000000000, -0.000000000000000000, -0.000000000000000000 ) ) ;
#19400 = AXIS2_PLACEMENT_3D ( 'NONE', #1302, #1396, #7522 ) ;
#19401 = EDGE_LOOP ( 'NONE', ( #11811, #2311, #3123, #2906 ) ) ;
#19402 = CARTESIAN_POINT ( 'NONE',  ( -6.165580000000000283, 0.000000000000000000, 7.500000000000000000 ) ) ;
#19403 = ORIENTED_EDGE ( 'NONE', *, *, #10701, .T. ) ;
#19404 = CARTESIAN_POINT ( 'NONE',  ( -12.72792206288791128, -12.72792205982779912, 17.41792500018031475 ) ) ;
#19405 = FACE_OUTER_BOUND ( 'NONE', #8695, .T. ) ;
#19406 = AXIS2_PLACEMENT_3D ( 'NONE', #8410, #359, #6925 ) ;
#19407 = ORIENTED_EDGE ( 'NONE', *, *, #9724, .T. ) ;
#19408 = VECTOR ( 'NONE', #3331, 1000.000000000000000 ) ;
#19409 = DIRECTION ( 'NONE',  ( -1.000000000000000000, 0.000000000000000000, 0.000000000000000000 ) ) ;
#19410 = EDGE_LOOP ( 'NONE', ( #12059, #7775 ) ) ;
#19411 = CARTESIAN_POINT ( 'NONE',  ( 0.2500000000000002220, 0.000000000000000000, 0.000000000000000000 ) ) ;
#19412 = CARTESIAN_POINT ( 'NONE',  ( 19.99999999999999645, -70.68211945903198057, 13.71269443944183841 ) ) ;
#19413 = VERTEX_POINT ( 'NONE', #19962 ) ;
#19414 = VERTEX_POINT ( 'NONE', #18601 ) ;
#19415 = LINE ( 'NONE', #441, #10023 ) ;
#19416 = VECTOR ( 'NONE', #8096, 1000.000000000000000 ) ;
#19417 = DIRECTION ( 'NONE',  ( -1.000000000000000000, 0.000000000000000000, 0.000000000000000000 ) ) ;
#19418 = CIRCLE ( 'NONE', #15018, 0.2500000000000002220 ) ;
#19419 = CIRCLE ( 'NONE', #10280, 27.60000000002759890 ) ;
#19420 = CARTESIAN_POINT ( 'NONE',  ( 19.99999999999999645, 53.26727847779537228, 48.44168704307649875 ) ) ;
#19421 = CIRCLE ( 'NONE', #16364, 65.24900000006525147 ) ;
#19423 = ORIENTED_EDGE ( 'NONE', *, *, #19776, .F. ) ;
#19422 = VECTOR ( 'NONE', #10836, 1000.000000000000000 ) ;
#19424 = AXIS2_PLACEMENT_3D ( 'NONE', #2914, #12458, #12675 ) ;
#19425 = CARTESIAN_POINT ( 'NONE',  ( 2.870125743571137811, 6.929096493489625530, 17.45661250018031296 ) ) ;
#19426 = CARTESIAN_POINT ( 'NONE',  ( 7.500000000000009770, -8.788009017158368372E-15, -2.786299999997682519 ) ) ;
#19427 = DIRECTION ( 'NONE',  ( -0.000000000000000000, -0.000000000000000000, 1.000000000000000000 ) ) ;
#19428 = CARTESIAN_POINT ( 'NONE',  ( 23.00000000000000000, 0.000000000000000000, -120.0000000000000142 ) ) ;
#19429 = ORIENTED_EDGE ( 'NONE', *, *, #1946, .F. ) ;
#19430 = FACE_OUTER_BOUND ( 'NONE', #14363, .T. ) ;
#19431 = CARTESIAN_POINT ( 'NONE',  ( -18.00000000043041126, -3.580422610670022543, 16.39691875018031908 ) ) ;
#19432 = DIRECTION ( 'NONE',  ( -1.000000000000000000, -0.000000000000000000, -0.000000000000000000 ) ) ;
#19433 = ORIENTED_EDGE ( 'NONE', *, *, #3208, .T. ) ;
#19434 = EDGE_CURVE ( 'NONE', #15450, #18079, #10029, .T. ) ;
#19435 = FACE_OUTER_BOUND ( 'NONE', #11382, .T. ) ;
#19436 = EDGE_LOOP ( 'NONE', ( #5137, #9058 ) ) ;
#19437 = DIRECTION ( 'NONE',  ( 0.000000000000000000, 0.000000000000000000, 1.000000000000000000 ) ) ;
#19438 = EDGE_CURVE ( 'NONE', #9449, #5396, #7653, .T. ) ;
#19439 = EDGE_LOOP ( 'NONE', ( #17735, #1606 ) ) ;
#19440 = CIRCLE ( 'NONE', #2858, 27.60000000002759890 ) ;
#19441 = CONICAL_SURFACE ( 'NONE', #20800, 4.000000000000000000, 1.047197551196595855 ) ;
#19442 = EDGE_CURVE ( 'NONE', #6220, #1870, #11049, .T. ) ;
#19443 = DIRECTION ( 'NONE',  ( -0.000000000000000000, -0.000000000000000000, 1.000000000000000000 ) ) ;
#19444 = DIRECTION ( 'NONE',  ( 0.000000000000000000, 0.2697967711570248839, -0.9629172873477991335 ) ) ;
#19445 = CARTESIAN_POINT ( 'NONE',  ( -10.32494394809439875, -4.276731812588566051, 20.61604725064743704 ) ) ;
#19446 = VERTEX_POINT ( 'NONE', #20067 ) ;
#19447 = DIRECTION ( 'NONE',  ( -0.000000000000000000, -0.000000000000000000, 1.000000000000000000 ) ) ;
#19448 = CARTESIAN_POINT ( 'NONE',  ( 6.165579999999996730, 0.000000000000000000, 0.000000000000000000 ) ) ;
#19449 = ORIENTED_EDGE ( 'NONE', *, *, #20065, .F. ) ;
#19450 = CARTESIAN_POINT ( 'NONE',  ( -7.632783294297951215E-14, -4.618802153517020948, -0.3572655899081733644 ) ) ;
#19451 = ADVANCED_FACE ( 'NONE', ( #5549 ), #2491, .F. ) ;
#19452 = AXIS2_PLACEMENT_3D ( 'NONE', #2058, #4280, #18698 ) ;
#19453 = CARTESIAN_POINT ( 'NONE',  ( -3.580422614997675002, -17.99999999956958163, 16.53433125018031191 ) ) ;
#19454 = DIRECTION ( 'NONE',  ( -1.000000000000000000, 0.000000000000000000, -0.000000000000000000 ) ) ;
#19455 = DIRECTION ( 'NONE',  ( 1.000000000000000000, 0.000000000000000000, 0.000000000000000000 ) ) ;
#19456 = ADVANCED_FACE ( 'NONE', ( #5759 ), #4179, .T. ) ;
#19457 = VERTEX_POINT ( 'NONE', #5879 ) ;
#19458 = EDGE_CURVE ( 'NONE', #14269, #5705, #897, .T. ) ;
#19459 = CARTESIAN_POINT ( 'NONE',  ( 30.00000000000000000, -85.00000000000000000, -45.00000000000000711 ) ) ;
#19460 = DIRECTION ( 'NONE',  ( 0.000000000000000000, 0.000000000000000000, -1.000000000000000000 ) ) ;
#19461 = EDGE_LOOP ( 'NONE', ( #20390, #11440, #1393, #15345 ) ) ;
#19462 = DIRECTION ( 'NONE',  ( -1.000000000000000000, 0.000000000000000000, 0.000000000000000000 ) ) ;
#19463 = DIRECTION ( 'NONE',  ( -1.000000000000000000, 0.000000000000000000, -0.000000000000000000 ) ) ;
#19464 = CARTESIAN_POINT ( 'NONE',  ( -1.491842754445842800, 7.500000000179346316, -5.437081249819685880 ) ) ;
#19465 = ADVANCED_FACE ( 'NONE', ( #2699 ), #9165, .T. ) ;
#19466 = ORIENTED_EDGE ( 'NONE', *, *, #14429, .F. ) ;
#19467 = CARTESIAN_POINT ( 'NONE',  ( 50.00000000000000000, 36.35083268962915781, -50.00000000000000000 ) ) ;
#19468 = VECTOR ( 'NONE', #14467, 1000.000000000000114 ) ;
#19469 = DIRECTION ( 'NONE',  ( -0.000000000000000000, -0.000000000000000000, -1.000000000000000000 ) ) ;
#19470 = APPLICATION_PROTOCOL_DEFINITION ( 'draft international standard', 'automotive_design', 1998, #12920 ) ;
#19471 = CARTESIAN_POINT ( 'NONE',  ( -18.00000000043041481, -3.580422610670022987, -19.39848124981969590 ) ) ;
#19472 = VERTEX_POINT ( 'NONE', #12784 ) ;
#19473 = DIRECTION ( 'NONE',  ( 0.000000000000000000, 0.000000000000000000, 1.000000000000000000 ) ) ;
#19474 = CARTESIAN_POINT ( 'NONE',  ( 0.000000000000000000, 0.000000000000000000, 0.000000000000000000 ) ) ;
#19475 = EDGE_CURVE ( 'NONE', #13495, #19867, #14256, .T. ) ;
#19476 = CARTESIAN_POINT ( 'NONE',  ( 8.382925371439627682, 12.54593441562639988, -10.20044816848092673 ) ) ;
#19477 = CIRCLE ( 'NONE', #18137, 80.00000000000000000 ) ;
#19478 = FACE_OUTER_BOUND ( 'NONE', #19882, .T. ) ;
#19479 = CIRCLE ( 'NONE', #5617, 2.099999999999990763 ) ;
#19480 = ORIENTED_EDGE ( 'NONE', *, *, #10644, .F. ) ;
#19481 = CARTESIAN_POINT ( 'NONE',  ( 0.000000000000000000, -19.38316218894168586, -61.87375713201008409 ) ) ;
#19482 = EDGE_CURVE ( 'NONE', #13947, #15185, #3587, .T. ) ;
#19483 = CARTESIAN_POINT ( 'NONE',  ( 9.015937996181842420E-10, 7.500000000000007994, 23.13245000018031661 ) ) ;
#19484 = DIRECTION ( 'NONE',  ( 0.000000000000000000, 0.000000000000000000, 1.000000000000000000 ) ) ;
#19485 = VERTEX_POINT ( 'NONE', #19022 ) ;
#19486 = FACE_OUTER_BOUND ( 'NONE', #5826, .T. ) ;
#19487 = ORIENTED_EDGE ( 'NONE', *, *, #12344, .F. ) ;
#19488 = CARTESIAN_POINT ( 'NONE',  ( 44.32616946416951720, -9.742112414153938360, -83.66536569035999094 ) ) ;
#19489 = CARTESIAN_POINT ( 'NONE',  ( -12.72792206288790950, -12.72792205982779556, 15.51332500018031268 ) ) ;
#19490 = ORIENTED_EDGE ( 'NONE', *, *, #19974, .F. ) ;
#19491 = VERTEX_POINT ( 'NONE', #20813 ) ;
#19492 = CARTESIAN_POINT ( 'NONE',  ( 49.19234958605026264, -1.326995226329893862, 84.99999999999998579 ) ) ;
#19493 = CIRCLE ( 'NONE', #16447, 27.60000000002759890 ) ;
#19494 = CARTESIAN_POINT ( 'NONE',  ( -6.177131623262581250, 0.000000000000000000, 0.000000000000000000 ) ) ;
#19495 =( LENGTH_UNIT ( ) NAMED_UNIT ( * ) SI_UNIT ( .MILLI., .METRE. ) );
#19496 = CARTESIAN_POINT ( 'NONE',  ( 9.999999999999998224, 10.74906464462217137, -71.19310085447958159 ) ) ;
#19497 = AXIS2_PLACEMENT_3D ( 'NONE', #7134, #17005, #13618 ) ;
#19498 = LINE ( 'NONE', #4881, #17664 ) ;
#19499 = CARTESIAN_POINT ( 'NONE',  ( 2.870125743571140475, 6.929096493489632635, 14.29651250018031661 ) ) ;
#19500 = CARTESIAN_POINT ( 'NONE',  ( 2.222972771497739419, 11.17563879704981922, 7.308171499713199459 ) ) ;
#19501 = CIRCLE ( 'NONE', #2291, 65.24900000006525147 ) ;
#19502 = CARTESIAN_POINT ( 'NONE',  ( 23.00000000000000000, 0.000000000000000000, -90.00000000000000000 ) ) ;
#19503 = DIRECTION ( 'NONE',  ( -1.000000000000000000, 0.000000000000000000, 0.000000000000000000 ) ) ;
#19504 = AXIS2_PLACEMENT_3D ( 'NONE', #18589, #9149, #13825 ) ;
#19505 = ORIENTED_EDGE ( 'NONE', *, *, #6924, .T. ) ;
#19506 = DIRECTION ( 'NONE',  ( -1.000000000000000000, 0.000000000000000000, -0.000000000000000000 ) ) ;
#19507 = CARTESIAN_POINT ( 'NONE',  ( -2.163827323447878234E-09, -18.00000000000000000, 6.814800000180313511 ) ) ;
#19508 = DIRECTION ( 'NONE',  ( 0.000000000000000000, 0.000000000000000000, 1.000000000000000000 ) ) ;
#19509 = ORIENTED_EDGE ( 'NONE', *, *, #13897, .T. ) ;
#19510 = CARTESIAN_POINT ( 'NONE',  ( 19.99999999999999645, -70.29359119158473845, -15.58239511117358944 ) ) ;
#19511 = VECTOR ( 'NONE', #12879, 1000.000000000000000 ) ;
#19512 = EDGE_LOOP ( 'NONE', ( #16718, #2978 ) ) ;
#19513 = VECTOR ( 'NONE', #686, 1000.000000000000000 ) ;
#19514 = CYLINDRICAL_SURFACE ( 'NONE', #4072, 205.0000000000000284 ) ;
#19515 = CARTESIAN_POINT ( 'NONE',  ( 45.22159793441011999, -8.673994507468384185, 84.62946326583127643 ) ) ;
#19516 = STYLED_ITEM ( 'NONE', ( #3185 ), #6131 ) ;
#19517 = EDGE_LOOP ( 'NONE', ( #4873, #3989 ) ) ;
#19518 = ORIENTED_EDGE ( 'NONE', *, *, #17128, .T. ) ;
#19519 = DIRECTION ( 'NONE',  ( -1.000000000000000000, -0.000000000000000000, -0.000000000000000000 ) ) ;
#19520 = ADVANCED_FACE ( 'NONE', ( #14368 ), #19134, .F. ) ;
#19521 = EDGE_CURVE ( 'NONE', #10081, #2829, #20855, .T. ) ;
#19522 = AXIS2_PLACEMENT_3D ( 'NONE', #16953, #7197, #8589 ) ;
#19523 = DIRECTION ( 'NONE',  ( -1.000000000000000000, 0.000000000000000000, -0.000000000000000000 ) ) ;
#19524 = AXIS2_PLACEMENT_3D ( 'NONE', #15143, #17048, #12276 ) ;
#19525 = VECTOR ( 'NONE', #18610, 1000.000000000000000 ) ;
#19526 = DIRECTION ( 'NONE',  ( 0.000000000000000000, 0.6310879443260485333, 0.7757112907044232397 ) ) ;
#19527 = ORIENTED_EDGE ( 'NONE', *, *, #11179, .F. ) ;
#19528 = VECTOR ( 'NONE', #2632, 1000.000000000000000 ) ;
#19529 = CARTESIAN_POINT ( 'NONE',  ( -1.491842756249031510, -7.499999999820660790, 12.44958125018031225 ) ) ;
#19530 = AXIS2_PLACEMENT_3D ( 'NONE', #18645, #12505, #12176 ) ;
#19531 = CARTESIAN_POINT ( 'NONE',  ( 6.359999999999999432, 10.52400000000000091, 0.000000000000000000 ) ) ;
#19532 = DIRECTION ( 'NONE',  ( -0.000000000000000000, -0.000000000000000000, 1.000000000000000000 ) ) ;
#19533 = CARTESIAN_POINT ( 'NONE',  ( 0.000000000000000000, -58.44960523466261293, 28.06621538408569805 ) ) ;
#19534 = ORIENTED_EDGE ( 'NONE', *, *, #3794, .T. ) ;
#19535 = LINE ( 'NONE', #16253, #10876 ) ;
#19536 = ORIENTED_EDGE ( 'NONE', *, *, #17633, .T. ) ;
#19537 = CARTESIAN_POINT ( 'NONE',  ( -10.19618095414378622, -15.25966316918061416, 15.21879375018031411 ) ) ;
#19538 = CARTESIAN_POINT ( 'NONE',  ( 50.00000000000000000, -49.99999999999999289, -71.93747284969079203 ) ) ;
#19539 = AXIS2_PLACEMENT_3D ( 'NONE', #11124, #7945, #19484 ) ;
#19540 = ORIENTED_EDGE ( 'NONE', *, *, #1348, .T. ) ;
#19541 = LINE ( 'NONE', #8103, #18734 ) ;
#19542 = ORIENTED_EDGE ( 'NONE', *, *, #20878, .F. ) ;
#19543 = CARTESIAN_POINT ( 'NONE',  ( 19.99999999999999645, 0.000000000000000000, 0.000000000000000000 ) ) ;
#19544 = CIRCLE ( 'NONE', #11094, 11.49999999999999645 ) ;
#19545 = ORIENTED_EDGE ( 'NONE', *, *, #11782, .F. ) ;
#19546 = AXIS2_PLACEMENT_3D ( 'NONE', #1211, #11053, #4693 ) ;
#19547 = CARTESIAN_POINT ( 'NONE',  ( 6.250000000000054179, 10.82531754730546147, 126.0000000000000000 ) ) ;
#19548 = LINE ( 'NONE', #5029, #15008 ) ;
#19549 = AXIS2_PLACEMENT_3D ( 'NONE', #15966, #9999, #11103 ) ;
#19550 = CARTESIAN_POINT ( 'NONE',  ( 5.663308650141532397, 13.67243654642775574, -14.30189558115846182 ) ) ;
#19551 = ADVANCED_FACE ( 'NONE', ( #18925 ), #17329, .F. ) ;
#19552 = EDGE_CURVE ( 'NONE', #14177, #17518, #561, .T. ) ;
#19553 = VERTEX_POINT ( 'NONE', #15736 ) ;
#19554 = DIRECTION ( 'NONE',  ( -1.000000000000000000, 0.000000000000000000, 0.000000000000000000 ) ) ;
#19555 = CIRCLE ( 'NONE', #3960, 80.00000000000000000 ) ;
#19556 = DIRECTION ( 'NONE',  ( -1.000000000000000000, -0.000000000000000000, -0.000000000000000000 ) ) ;
#19557 = VERTEX_POINT ( 'NONE', #4500 ) ;
#19558 = CARTESIAN_POINT ( 'NONE',  ( -10.00000000000000000, 0.000000000000000000, 0.000000000000000000 ) ) ;
#19559 = CARTESIAN_POINT ( 'NONE',  ( 6.888301784570728614, 16.62983158437510056, 21.54136250018031618 ) ) ;
#19560 = DIRECTION ( 'NONE',  ( -1.000000000000000000, 0.000000000000000000, -0.000000000000000000 ) ) ;
#19561 = CARTESIAN_POINT ( 'NONE',  ( -30.00000000000000000, -30.00000000000000000, -120.0000000000000142 ) ) ;
#19562 = EDGE_CURVE ( 'NONE', #2697, #11465, #12413, .T. ) ;
#19563 = ORIENTED_EDGE ( 'NONE', *, *, #19081, .T. ) ;
#19564 = FACE_BOUND ( 'NONE', #20165, .T. ) ;
#19565 = EDGE_LOOP ( 'NONE', ( #6392, #283, #17122, #13813 ) ) ;
#19566 = CARTESIAN_POINT ( 'NONE',  ( 3.600000000000060485, 10.82531754730546147, 129.0000000000000000 ) ) ;
#19567 = DIRECTION ( 'NONE',  ( 0.000000000000000000, 0.000000000000000000, -1.000000000000000000 ) ) ;
#19568 = CARTESIAN_POINT ( 'NONE',  ( 16.62983158437509346, -6.888301784570737496, -25.13198749981969371 ) ) ;
#19569 = ORIENTED_EDGE ( 'NONE', *, *, #1484, .F. ) ;
#19570 = FACE_OUTER_BOUND ( 'NONE', #157, .T. ) ;
#19571 = DIRECTION ( 'NONE',  ( 0.7071067811865445751, 0.4413865154835797666, -0.5524291302504493739 ) ) ;
#19572 = CARTESIAN_POINT ( 'NONE',  ( 12.72792206288791128, 12.72792205982780267, -6.144574999819692351 ) ) ;
#19573 = EDGE_CURVE ( 'NONE', #4727, #1571, #10377, .T. ) ;
#19574 = ORIENTED_EDGE ( 'NONE', *, *, #9984, .T. ) ;
#19575 = B_SPLINE_CURVE_WITH_KNOTS ( 'NONE', 3,
 ( #19253, #6624, #7917, #6323, #4633, #11502 ),
 .UNSPECIFIED., .F., .F.,
 ( 4, 2, 4 ),
 ( 0.006456566858647395761, 0.007625406818786647362, 0.008794246778925899830 ),
 .UNSPECIFIED. ) ;
#19576 = EDGE_CURVE ( 'NONE', #10139, #9276, #13426, .T. ) ;
#19577 = DIRECTION ( 'NONE',  ( 0.000000000000000000, 0.000000000000000000, -1.000000000000000000 ) ) ;
#19578 = FACE_OUTER_BOUND ( 'NONE', #14316, .T. ) ;
#19579 = CARTESIAN_POINT ( 'NONE',  ( -2.943691925285395694, 14.79893867793683349, -11.37857316848092637 ) ) ;
#19580 = DIRECTION ( 'NONE',  ( -1.000000000000000000, 0.000000000000000000, 0.000000000000000000 ) ) ;
#19581 = EDGE_CURVE ( 'NONE', #10704, #1189, #15937, .T. ) ;
#19582 = PRODUCT_DEFINITION ( 'UNKNOWN', '', #13716, #7075 ) ;
#19583 = EDGE_LOOP ( 'NONE', ( #18285, #14085, #14022, #17034, #7021, #12492 ) ) ;
#19584 = DIRECTION ( 'NONE',  ( -1.000000000000000000, 0.000000000000000000, 0.000000000000000000 ) ) ;
#19585 = DIRECTION ( 'NONE',  ( 0.000000000000000000, 0.000000000000000000, 1.000000000000000000 ) ) ;
#19586 = CARTESIAN_POINT ( 'NONE',  ( 33.92785236135936344, -27.95564457753036436, 68.35308193655099274 ) ) ;
#19587 = ORIENTED_EDGE ( 'NONE', *, *, #12796, .F. ) ;
#19588 = DIRECTION ( 'NONE',  ( 1.000000000000000000, 0.000000000000000000, 0.000000000000000000 ) ) ;
#19589 = VERTEX_POINT ( 'NONE', #3113 ) ;
#19590 = DIRECTION ( 'NONE',  ( -1.000000000000000000, -0.000000000000000000, -0.000000000000000000 ) ) ;
#19591 = CARTESIAN_POINT ( 'NONE',  ( -30.00000000000000000, -3.649167310370807105, -90.00000000000000000 ) ) ;
#19592 = VERTEX_POINT ( 'NONE', #6081 ) ;
#19593 = EDGE_CURVE ( 'NONE', #1684, #1429, #9383, .T. ) ;
#19594 = ORIENTED_EDGE ( 'NONE', *, *, #9539, .T. ) ;
#19595 = DIRECTION ( 'NONE',  ( 0.000000000000000000, 0.000000000000000000, -1.000000000000000000 ) ) ;
#19596 = ADVANCED_FACE ( 'NONE', ( #1545 ), #1337, .T. ) ;
#19597 = CARTESIAN_POINT ( 'NONE',  ( 30.00000000000000000, -99.99999999999998579, 54.09999999999998721 ) ) ;
#19598 =( LENGTH_UNIT ( ) NAMED_UNIT ( * ) SI_UNIT ( .MILLI., .METRE. ) );
#19599 = CARTESIAN_POINT ( 'NONE',  ( 19.99999999999999645, -63.85430960833482317, 16.34407078397855528 ) ) ;
#19600 = ADVANCED_FACE ( 'NONE', ( #20604 ), #16052, .T. ) ;
#19601 = CARTESIAN_POINT ( 'NONE',  ( 19.99999999999999645, 71.76067541710858677, -5.865617076723870227 ) ) ;
#19602 = CARTESIAN_POINT ( 'NONE',  ( -4.248408729364580694, 6.358192988180020322, 22.24885625018031732 ) ) ;
#19603 = CARTESIAN_POINT ( 'NONE',  ( -4.276731815070945686, -10.32494394706615637, 12.31520274971320106 ) ) ;
#19604 = DIRECTION ( 'NONE',  ( 0.000000000000000000, -0.000000000000000000, 1.000000000000000000 ) ) ;
#19605 = CARTESIAN_POINT ( 'NONE',  ( 30.00000000000000000, -122.0000000000000000, -6.368163355566234804E-15 ) ) ;
#19606 = ORIENTED_EDGE ( 'NONE', *, *, #2981, .F. ) ;
#19607 = LINE ( 'NONE', #9961, #2444 ) ;
#19608 = CARTESIAN_POINT ( 'NONE',  ( -10.19618095047498052, 15.25966317163203101, 20.06870625018031262 ) ) ;
#19609 = LINE ( 'NONE', #8271, #17763 ) ;
#19610 = ORIENTED_EDGE ( 'NONE', *, *, #7411, .T. ) ;
#19611 = CARTESIAN_POINT ( 'NONE',  ( -3.345653888883671989, 2.687187980154694511, -0.1391502195351393412 ) ) ;
#19612 = EDGE_LOOP ( 'NONE', ( #6495, #8351, #3703, #15932 ) ) ;
#19613 = FACE_OUTER_BOUND ( 'NONE', #8779, .T. ) ;
#19614 = DIRECTION ( 'NONE',  ( 1.000000000000000000, -0.000000000000000000, 0.000000000000000000 ) ) ;
#19615 = VERTEX_POINT ( 'NONE', #7997 ) ;
#19616 = ORIENTED_EDGE ( 'NONE', *, *, #7060, .F. ) ;
#19617 = DIRECTION ( 'NONE',  ( -1.000000000000000000, 0.000000000000000000, 0.000000000000000000 ) ) ;
#19618 =( NAMED_UNIT ( * ) SI_UNIT ( $, .STERADIAN. ) SOLID_ANGLE_UNIT ( ) );
#19619 = CARTESIAN_POINT ( 'NONE',  ( 19.99999999999999645, 20.34307325858883431, -69.06634035770284186 ) ) ;
#19620 = CARTESIAN_POINT ( 'NONE',  ( 0.000000000000000000, 0.000000000000000000, -68.00000000000000000 ) ) ;
#19621 = ORIENTED_EDGE ( 'NONE', *, *, #4964, .T. ) ;
#19622 = CARTESIAN_POINT ( 'NONE',  ( -7.500000000179339210, -1.491842754445842800, 14.21676875018031261 ) ) ;
#19623 = CARTESIAN_POINT ( 'NONE',  ( 6.249999999999902300, -10.82531754730554496, 46.00000000000000711 ) ) ;
#19624 = CARTESIAN_POINT ( 'NONE',  ( 19.99999999999999645, 35.35772184876955038, -54.34979580218157480 ) ) ;
#19625 = DIRECTION ( 'NONE',  ( 1.000000000000000000, 0.000000000000000000, 0.000000000000000000 ) ) ;
#19626 = CARTESIAN_POINT ( 'NONE',  ( -12.50000000000000533, 0.000000000000000000, 43.00000000000000000 ) ) ;
#19627 = ORIENTED_EDGE ( 'NONE', *, *, #15093, .F. ) ;
#19628 = EDGE_CURVE ( 'NONE', #20371, #200, #1919, .T. ) ;
#19629 = CYLINDRICAL_SURFACE ( 'NONE', #11878, 17.50000000000000355 ) ;
#19630 = EDGE_LOOP ( 'NONE', ( #16509, #19796 ) ) ;
#19631 = DIRECTION ( 'NONE',  ( -0.000000000000000000, -0.000000000000000000, 1.000000000000000000 ) ) ;
#19632 = DIRECTION ( 'NONE',  ( -1.000000000000000000, 0.000000000000000000, 0.000000000000000000 ) ) ;
#19633 = CIRCLE ( 'NONE', #18983, 27.60000000002759535 ) ;
#19634 = VERTEX_POINT ( 'NONE', #20503 ) ;
#19635 = CARTESIAN_POINT ( 'NONE',  ( 19.99999999999999645, -63.85430960833482317, -11.25592921604904539 ) ) ;
#19636 = ORIENTED_EDGE ( 'NONE', *, *, #3388, .F. ) ;
#19637 = CARTESIAN_POINT ( 'NONE',  ( 50.00000000000000000, -164.9999999999999716, 90.00000000000001421 ) ) ;
#19638 = LINE ( 'NONE', #5115, #13465 ) ;
#19639 = ORIENTED_EDGE ( 'NONE', *, *, #8157, .T. ) ;
#19640 = AXIS2_PLACEMENT_3D ( 'NONE', #14048, #4282, #18917 ) ;
#19641 = DIRECTION ( 'NONE',  ( 1.000000000000000000, 0.000000000000000000, 0.000000000000000000 ) ) ;
#19642 = DIRECTION ( 'NONE',  ( 0.000000000000000000, 0.000000000000000000, -1.000000000000000000 ) ) ;
#19643 = AXIS2_PLACEMENT_3D ( 'NONE', #2260, #13596, #2155 ) ;
#19644 = CARTESIAN_POINT ( 'NONE',  ( 7.902369978624329327, 7.902369976724401113, 15.31448475064743242 ) ) ;
#19645 = VERTEX_POINT ( 'NONE', #5983 ) ;
#19646 = CYLINDRICAL_SURFACE ( 'NONE', #6932, 34.99999999999999289 ) ;
#19647 = DIRECTION ( 'NONE',  ( 0.000000000000000000, 0.000000000000000000, 1.000000000000000000 ) ) ;
#19648 = VERTEX_POINT ( 'NONE', #12457 ) ;
#19649 = FACE_OUTER_BOUND ( 'NONE', #6722, .T. ) ;
#19650 = ORIENTED_EDGE ( 'NONE', *, *, #5630, .T. ) ;
#19651 = ADVANCED_FACE ( 'NONE', ( #14161 ), #15795, .T. ) ;
#19652 = CARTESIAN_POINT ( 'NONE',  ( -2.163827323447878234E-09, -18.00000000000000000, 16.23980000018031333 ) ) ;
#19653 = DIRECTION ( 'NONE',  ( 0.000000000000000000, 0.000000000000000000, 1.000000000000000000 ) ) ;
#19654 = DIRECTION ( 'NONE',  ( -1.000000000000000000, 0.000000000000000000, 0.000000000000000000 ) ) ;
#19655 = VERTEX_POINT ( 'NONE', #3626 ) ;
#19656 = PLANE ( 'NONE',  #15126 ) ;
#19657 = AXIS2_PLACEMENT_3D ( 'NONE', #5823, #20656, #2756 ) ;
#19658 = ORIENTED_EDGE ( 'NONE', *, *, #1368, .T. ) ;
#19659 = ADVANCED_FACE ( 'NONE', ( #2040 ), #8296, .F. ) ;
#19660 = DIRECTION ( 'NONE',  ( -1.000000000000000000, 0.000000000000000000, -0.000000000000000000 ) ) ;
#19661 = CARTESIAN_POINT ( 'NONE',  ( -6.929096494179684207, -2.870125741905212635, -17.51286249981968979 ) ) ;
#19662 = ORIENTED_EDGE ( 'NONE', *, *, #9877, .T. ) ;
#19663 = CARTESIAN_POINT ( 'NONE',  ( 19.99999999999999645, 51.96384592647198986, 49.83732252579632416 ) ) ;
#19664 = DIRECTION ( 'NONE',  ( -1.000000000000000000, -0.000000000000000000, -0.000000000000000000 ) ) ;
#19665 = CARTESIAN_POINT ( 'NONE',  ( -12.50000000000000888, 1.703253897049806897E-13, -39.99999999999999289 ) ) ;
#19666 =( BOUNDED_CURVE ( )  B_SPLINE_CURVE ( 2, ( #710, #5270, #18525, #5470, #10467, #300, #16605, #2308, #3573, #11743, #10150, #6751, #18307, #18212, #13229, #8656, #2197 ),
 .UNSPECIFIED., .F., .T. ) 
 B_SPLINE_CURVE_WITH_KNOTS ( ( 3, 2, 2, 2, 2, 2, 2, 2, 3 ),
 ( 0.000000000000000000, 0.01250000000048139860, 0.02500000000096279720, 0.03750000000144419060, 0.05000000000192559441, 0.06250000000240699127, 0.07500000000288838120, 0.08750000000336977113, 0.1000000000038511888 ),
 .UNSPECIFIED. ) 
 CURVE ( )  GEOMETRIC_REPRESENTATION_ITEM ( )  RATIONAL_B_SPLINE_CURVE ( ( 1.000000000000000000, 0.9807852804032304306, 1.000000000000000000, 0.9807852804032304306, 1.000000000000000000, 0.9807852804032304306, 1.000000000000000000, 0.9807852804032304306, 1.000000000000000000, 0.9807852804032304306, 1.000000000000000000, 0.9807852804032304306, 1.000000000000000000, 0.9807852804032304306, 1.000000000000000000, 0.9807852803973104994, 1.000000000005919931 ) ) 
 REPRESENTATION_ITEM ( '' )  );
#19667 = CARTESIAN_POINT ( 'NONE',  ( -8.382925368423274293, 12.54593441764187745, 12.50044816884154564 ) ) ;
#19668 = AXIS2_PLACEMENT_3D ( 'NONE', #5287, #5485, #5699 ) ;
#19670 = VERTEX_POINT ( 'NONE', #10100 ) ;
#19669 = CIRCLE ( 'NONE', #17986, 5.000000000000004441 ) ;
#19671 = CARTESIAN_POINT ( 'NONE',  ( -2.870125741905210415, 6.929096494179677990, 6.853487500180309056 ) ) ;
#19672 = AXIS2_PLACEMENT_3D ( 'NONE', #2203, #6963, #3778 ) ;
#19673 = CARTESIAN_POINT ( 'NONE',  ( 2.943691925285397470, -14.79893867793683349, 2.758926831519074696 ) ) ;
#19674 = ORIENTED_EDGE ( 'NONE', *, *, #2403, .F. ) ;
#19675 =( REPRESENTATION_RELATIONSHIP ('NONE','NONE', #13739, #20346 ) REPRESENTATION_RELATIONSHIP_WITH_TRANSFORMATION ( #20193 )SHAPE_REPRESENTATION_RELATIONSHIP( ) );
#19676 = CIRCLE ( 'NONE', #7147, 7.500000000000000000 ) ;
#19677 = DIRECTION ( 'NONE',  ( 0.000000000000000000, 0.4999999999999993339, -0.8660254037844390407 ) ) ;
#19678 = DIRECTION ( 'NONE',  ( 1.000000000000000000, 1.836909530733573776E-16, 0.000000000000000000 ) ) ;
#19679 = CARTESIAN_POINT ( 'NONE',  ( -24.99999999999999289, -160.0000000000000000, 0.000000000000000000 ) ) ;
#19680 = EDGE_LOOP ( 'NONE', ( #17167, #1731, #1207, #1093, #11024, #12555, #6707, #11634, #7894, #17181, #15060, #17447, #18923, #12232, #19271, #13060, #18138, #3967, #20170, #13731, #19386, #6594, #9007, #18466, #9247, #18264, #4261, #2127, #12664, #3804, #7307, #9061, #9330, #14474, #3941, #9886, #5971, #6548, #9573, #576, #12645, #19842, #10771, #18331, #13069, #2676, #17603, #491, #14665, #6345, #3011, #18527, #8277, #19674, #15543, #17521, #11890, #10866, #3425, #1329, #19972, #20559, #2656, #2859, #16304, #18075, #8737, #1019, #20599, #6213, #10536, #772, #20636, #3959, #2171, #11390, #12295, #10288, #42, #4243, #13522, #3555, #7281, #11252, #15996, #3973, #4286, #5691, #7568, #11951, #13861, #17862, #941, #14786, #10233, #8323, #535, #4237, #1199, #749, #3853, #625, #4189, #8402, #2202, #12959, #7235, #19213, #14591, #73, #13471, #12927, #12302, #2181, #6404, #10325, #9771, #11125, #11906, #596, #3389, #18425, #7670, #8142, #1890, #4516, #15659, #15812, #14049, #17708, #14985, #16047, #16149, #3932, #14771, #14108, #14711, #10157, #16741, #6293, #13192, #4860, #18523, #9178, #6473, #12030, #5301, #20873, #13830, #1004, #10206, #18156, #2810, #4115, #2867, #20699, #3312, #12450, #13914, #18581, #460, #20099, #9169, #7328, #3625, #4496, #15372, #20548, #9736, #7622, #14339, #15527, #144, #20292, #15712, #4830, #18603, #11469, #14075, #2990, #20085, #18236, #6462, #10261, #9941, #17572, #1576, #11846, #16720 ) ) ;
#19681 = AXIS2_PLACEMENT_3D ( 'NONE', #17448, #19240, #20610 ) ;
#19682 = EDGE_CURVE ( 'NONE', #645, #12045, #3521, .T. ) ;
#19683 = CARTESIAN_POINT ( 'NONE',  ( 0.000000000000000000, -56.42118728228177105, 32.77318456705422278 ) ) ;
#19684 = CIRCLE ( 'NONE', #5457, 27.60000000002759890 ) ;
#19685 = VERTEX_POINT ( 'NONE', #16254 ) ;
#19686 = CYLINDRICAL_SURFACE ( 'NONE', #741, 27.60000000002759890 ) ;
#19687 = CARTESIAN_POINT ( 'NONE',  ( -3.580422610670017658, 18.00000000043040771, 18.75316875018031126 ) ) ;
#19688 = EDGE_CURVE ( 'NONE', #2782, #18871, #1258, .T. ) ;
#19689 = EDGE_LOOP ( 'NONE', ( #3674, #3667, #16209, #13454 ) ) ;
#19690 = CIRCLE ( 'NONE', #8857, 65.24900000006525147 ) ;
#19691 = VERTEX_POINT ( 'NONE', #14871 ) ;
#19692 = CARTESIAN_POINT ( 'NONE',  ( -8.500000000000000000, 0.000000000000000000, -90.00000000000000000 ) ) ;
#19693 = CARTESIAN_POINT ( 'NONE',  ( 1.040949779275250179E-14, -85.00000000000000000, 19.00000000000000000 ) ) ;
#19694 = FACE_OUTER_BOUND ( 'NONE', #2378, .T. ) ;
#19695 = EDGE_CURVE ( 'NONE', #6425, #16884, #251, .T. ) ;
#19696 =( LENGTH_UNIT ( ) NAMED_UNIT ( * ) SI_UNIT ( .MILLI., .METRE. ) );
#19697 = DIRECTION ( 'NONE',  ( -0.000000000000000000, -0.000000000000000000, 1.000000000000000000 ) ) ;
#19698 = DIRECTION ( 'NONE',  ( -1.000000000000000000, 0.000000000000000000, -0.000000000000000000 ) ) ;
#19699 = CARTESIAN_POINT ( 'NONE',  ( 7.500000000000007994, -9.015933403756345817E-10, 25.48870000018031590 ) ) ;
#19700 = AXIS2_PLACEMENT_3D ( 'NONE', #20222, #18431, #12277 ) ;
#19701 = AXIS2_PLACEMENT_3D ( 'NONE', #11861, #8579, #20010 ) ;
#19702 = CARTESIAN_POINT ( 'NONE',  ( 2.222972768810837163, -11.17563879758427525, 11.43160899971319822 ) ) ;
#19703 = CIRCLE ( 'NONE', #14651, 11.17999999999999439 ) ;
#19704 = DIRECTION ( 'NONE',  ( 0.000000000000000000, 0.000000000000000000, -1.000000000000000000 ) ) ;
#19705 = DIRECTION ( 'NONE',  ( 0.000000000000000000, 0.8169698930104432044, -0.5766803221148655290 ) ) ;
#19706 = EDGE_CURVE ( 'NONE', #2775, #7789, #14115, .T. ) ;
#19707 = ORIENTED_EDGE ( 'NONE', *, *, #11217, .T. ) ;
#19708 = CARTESIAN_POINT ( 'NONE',  ( 19.99999999999999645, 0.000000000000000000, 0.000000000000000000 ) ) ;
#19709 = CARTESIAN_POINT ( 'NONE',  ( -6.888301784570738384, -16.62983158437509346, 16.82886250018031404 ) ) ;
#19710 = DIRECTION ( 'NONE',  ( -1.000000000000000000, 0.000000000000000000, 0.000000000000000000 ) ) ;
#19711 = CIRCLE ( 'NONE', #19385, 72.00000000007199219 ) ;
#19712 = VERTEX_POINT ( 'NONE', #18056 ) ;
#19713 = EDGE_CURVE ( 'NONE', #13515, #10665, #4959, .T. ) ;
#19714 = DIRECTION ( 'NONE',  ( -1.000000000000000000, -0.000000000000000000, -0.000000000000000000 ) ) ;
#19715 = VERTEX_POINT ( 'NONE', #9991 ) ;
#19716 = CARTESIAN_POINT ( 'NONE',  ( 2.500000000000000000, -2.357898499370432610, 3.252606517456513302E-15 ) ) ;
#19717 = DIRECTION ( 'NONE',  ( -1.000000000000000000, -0.000000000000000000, -0.000000000000000000 ) ) ;
#19718 = EDGE_CURVE ( 'NONE', #4533, #1320, #16136, .T. ) ;
#19719 = ORIENTED_EDGE ( 'NONE', *, *, #8185, .T. ) ;
#19720 = ORIENTED_EDGE ( 'NONE', *, *, #13401, .F. ) ;
#19721 = CYLINDRICAL_SURFACE ( 'NONE', #18146, 14.49999999999999822 ) ;
#19722 = AXIS2_PLACEMENT_3D ( 'NONE', #2185, #13120, #8533 ) ;
#19723 = CIRCLE ( 'NONE', #20730, 4.250000000000000000 ) ;
#19724 = ADVANCED_FACE ( 'NONE', ( #6704 ), #11697, .F. ) ;
#19725 = AXIS2_PLACEMENT_3D ( 'NONE', #8155, #4986, #11649 ) ;
#19726 = CIRCLE ( 'NONE', #10597, 65.24900000006526568 ) ;
#19727 = SHAPE_REPRESENTATION_RELATIONSHIP ( 'NONE' , 'NONE' ,  #9416, #7446 ) ;
#19728 = DIRECTION ( 'NONE',  ( -1.000000000000000000, -0.000000000000000000, -0.000000000000000000 ) ) ;
#19729 = CARTESIAN_POINT ( 'NONE',  ( 30.00000000000000711, -40.00000000000001421, -120.0000000000000142 ) ) ;
#19730 = VECTOR ( 'NONE', #17284, 1000.000000000000000 ) ;
#19731 = CARTESIAN_POINT ( 'NONE',  ( -1.491842754445841246, 7.500000000179339210, 7.148018750180312963 ) ) ;
#19732 = CYLINDRICAL_SURFACE ( 'NONE', #18634, 2.649999999999993694 ) ;
#19733 = FACE_OUTER_BOUND ( 'NONE', #903, .T. ) ;
#19734 = TOROIDAL_SURFACE ( 'NONE', #12989, 4.000000000000000000, 0.2500000000000000000 ) ;
#19735 = CARTESIAN_POINT ( 'NONE',  ( 0.000000000000000000, 0.000000000000000000, -5.574599999999999334 ) ) ;
#19736 = CARTESIAN_POINT ( 'NONE',  ( 6.359999999999999432, -10.52399999999998670, 1.288818291422673781E-15 ) ) ;
#19737 = CIRCLE ( 'NONE', #20057, 27.60000000002759890 ) ;
#19738 = ADVANCED_FACE ( 'NONE', ( #14313, #9524, #15784, #17595 ), #20754, .F. ) ;
#19739 = ORIENTED_EDGE ( 'NONE', *, *, #9798, .F. ) ;
#19740 = PLANE ( 'NONE',  #4114 ) ;
#19741 = EDGE_LOOP ( 'NONE', ( #17099, #6130, #19225, #4199 ) ) ;
#19742 = CARTESIAN_POINT ( 'NONE',  ( -6.888301784570738384, -16.62983158437509346, 14.92426250018031375 ) ) ;
#19743 = FACE_OUTER_BOUND ( 'NONE', #2885, .T. ) ;
#19744 = VERTEX_POINT ( 'NONE', #15677 ) ;
#19745 = FACE_OUTER_BOUND ( 'NONE', #3197, .T. ) ;
#19746 = ORIENTED_EDGE ( 'NONE', *, *, #14533, .T. ) ;
#19747 = LINE ( 'NONE', #11389, #18288 ) ;
#19748 = DIRECTION ( 'NONE',  ( -1.000000000000000000, -0.000000000000000000, 0.000000000000000000 ) ) ;
#19749 = ORIENTED_EDGE ( 'NONE', *, *, #11217, .F. ) ;
#19750 = VECTOR ( 'NONE', #1705, 1000.000000000000000 ) ;
#19751 = DIRECTION ( 'NONE',  ( 0.000000000000000000, 0.000000000000000000, -1.000000000000000000 ) ) ;
#19752 = DIRECTION ( 'NONE',  ( 0.000000000000000000, 0.000000000000000000, 1.000000000000000000 ) ) ;
#19753 = CIRCLE ( 'NONE', #1167, 2.500000000000002220 ) ;
#19754 = ADVANCED_FACE ( 'NONE', ( #12725 ), #1179, .F. ) ;
#19755 = DIRECTION ( 'NONE',  ( -1.000000000000000000, -0.000000000000000000, -0.000000000000000000 ) ) ;
#19756 = CARTESIAN_POINT ( 'NONE',  ( -7.902369978624331104, -7.902369976724401113, 1.176984750647428468 ) ) ;
#19757 = ORIENTED_EDGE ( 'NONE', *, *, #5069, .F. ) ;
#19758 = DIRECTION ( 'NONE',  ( 1.202124453834178081E-10, 1.000000000000000000, 0.000000000000000000 ) ) ;
#19759 = ORIENTED_EDGE ( 'NONE', *, *, #4275, .F. ) ;
#19760 = CARTESIAN_POINT ( 'NONE',  ( -2.000000000000022649, -3.464101615137742396, 0.000000000000000000 ) ) ;
#19761 = AXIS2_PLACEMENT_3D ( 'NONE', #5897, #16176, #8013 ) ;
#19762 = ORIENTED_EDGE ( 'NONE', *, *, #9696, .F. ) ;
#19763 = CARTESIAN_POINT ( 'NONE',  ( 15.25966316918061416, -10.19618095414378622, 5.342143750180314399 ) ) ;
#19764 = CARTESIAN_POINT ( 'NONE',  ( 9.999999999999998224, -0.9548212943360466776, -71.99366858485717557 ) ) ;
#19765 = CARTESIAN_POINT ( 'NONE',  ( 6.250000000000054179, 10.82531754730546147, 43.00000000000000000 ) ) ;
#19766 = CIRCLE ( 'NONE', #6230, 2.649999999999999467 ) ;
#19767 = ORIENTED_EDGE ( 'NONE', *, *, #17762, .F. ) ;
#19768 = AXIS2_PLACEMENT_3D ( 'NONE', #16255, #10101, #17952 ) ;
#19769 = CARTESIAN_POINT ( 'NONE',  ( 45.76122707727121508, -127.3290820621008947, -85.00000000000000000 ) ) ;
#19770 = ORIENTED_EDGE ( 'NONE', *, *, #19370, .F. ) ;
#19771 = DIRECTION ( 'NONE',  ( 1.000000000000000000, 0.000000000000000000, 0.000000000000000000 ) ) ;
#19772 = VECTOR ( 'NONE', #8387, 1000.000000000000000 ) ;
#19773 = ORIENTED_EDGE ( 'NONE', *, *, #8438, .F. ) ;
#19774 = CARTESIAN_POINT ( 'NONE',  ( -18.00000000000000000, 2.204364238465235428E-15, -130.0000000000000000 ) ) ;
#19775 = ADVANCED_FACE ( 'NONE', ( #20651 ), #6133, .F. ) ;
#19776 = EDGE_CURVE ( 'NONE', #10364, #4710, #915, .T. ) ;
#19777 = CARTESIAN_POINT ( 'NONE',  ( 0.000000000000000000, 0.000000000000000000, 0.000000000000000000 ) ) ;
#19778 = APPLICATION_PROTOCOL_DEFINITION ( 'draft international standard', 'automotive_design', 1998, #189 ) ;
#19779 = CARTESIAN_POINT ( 'NONE',  ( -10.46442989454075878, -10.46442989202484242, 19.27466691884154670 ) ) ;
#19780 = VERTEX_POINT ( 'NONE', #4235 ) ;
#19781 = AXIS2_PLACEMENT_3D ( 'NONE', #6911, #10199, #12001 ) ;
#19782 = CARTESIAN_POINT ( 'NONE',  ( 0.000000000000000000, -8.857208570069305509, -71.45313048675095047 ) ) ;
#19783 = CARTESIAN_POINT ( 'NONE',  ( 19.99999999999999645, 71.89099403602354244, -3.960426305689046522 ) ) ;
#19784 = CARTESIAN_POINT ( 'NONE',  ( -15.25966316918061416, 10.19618095414378445, 17.57504375018031340 ) ) ;
#19785 = VERTEX_POINT ( 'NONE', #17176 ) ;
#19786 = ORIENTED_EDGE ( 'NONE', *, *, #18651, .F. ) ;
#19787 = CARTESIAN_POINT ( 'NONE',  ( 0.000000000000000000, 56.42118728228155788, 32.77318456705461358 ) ) ;
#19788 = CARTESIAN_POINT ( 'NONE',  ( -62.49999999999999289, -120.0000000000000142, 0.000000000000000000 ) ) ;
#19789 = EDGE_LOOP ( 'NONE', ( #19158, #8498, #15219, #6551 ) ) ;
#19790 = CARTESIAN_POINT ( 'NONE',  ( -1.491842756249033286, -7.499999999820668783, 9.289481250180315897 ) ) ;
#19791 = ORIENTED_EDGE ( 'NONE', *, *, #13261, .T. ) ;
#19792 = CARTESIAN_POINT ( 'NONE',  ( 85.00002539999999840, 0.000000000000000000, 0.000000000000000000 ) ) ;
#19793 = CARTESIAN_POINT ( 'NONE',  ( -6.888301784570736608, -16.62983158437509346, 14.92426250018031020 ) ) ;
#19794 = ADVANCED_BREP_SHAPE_REPRESENTATION ( '', ( #10511, #12461 ), #5631 ) ;
#19795 = ORIENTED_EDGE ( 'NONE', *, *, #6479, .F. ) ;
#19796 = ORIENTED_EDGE ( 'NONE', *, *, #8285, .T. ) ;
#19797 = CARTESIAN_POINT ( 'NONE',  ( 2.500000000000000000, -2.357898499370432610, 3.252606517456513302E-15 ) ) ;
#19798 = DIRECTION ( 'NONE',  ( 0.000000000000000000, 0.000000000000000000, 1.000000000000000000 ) ) ;
#19799 = CARTESIAN_POINT ( 'NONE',  ( 50.00000000000000000, 36.35083268962915781, -50.00000000000000000 ) ) ;
#19800 = ORIENTED_EDGE ( 'NONE', *, *, #19830, .F. ) ;
#19801 = CARTESIAN_POINT ( 'NONE',  ( -2.163827323447878648E-09, -18.00000000000000355, 16.23980000018031333 ) ) ;
#19802 = UNCERTAINTY_MEASURE_WITH_UNIT (LENGTH_MEASURE( 1.000000000000000082E-05 ), #20023, 'distance_accuracy_value', 'NONE');
#19803 = CARTESIAN_POINT ( 'NONE',  ( 0.000000000000000000, 44.69367065308645692, 56.44887778834763026 ) ) ;
#19804 = CARTESIAN_POINT ( 'NONE',  ( 7.902369976724399336, -7.902369978624331104, -20.02926524935257646 ) ) ;
#19805 = EDGE_CURVE ( 'NONE', #2608, #5687, #20875, .T. ) ;
#19806 = CIRCLE ( 'NONE', #10690, 2.649999999999987477 ) ;
#19807 = CARTESIAN_POINT ( 'NONE',  ( -10.32494394809439164, -4.276731812588563386, -14.78167225028680676 ) ) ;
#19808 = PRODUCT_DEFINITION_SHAPE ( 'NONE', 'NONE',  #20961 ) ;
#19809 = EDGE_CURVE ( 'NONE', #6701, #16060, #6972, .T. ) ;
#19810 = DIRECTION ( 'NONE',  ( -1.000000000000000000, -0.000000000000000000, -0.000000000000000000 ) ) ;
#19811 = CARTESIAN_POINT ( 'NONE',  ( 0.000000000000000000, 0.000000000000000000, -120.0000000000000142 ) ) ;
#19812 = VERTEX_POINT ( 'NONE', #17805 ) ;
#19813 = CARTESIAN_POINT ( 'NONE',  ( 19.99999999999999645, 35.35772184876955038, -54.34979580218157480 ) ) ;
#19814 = CARTESIAN_POINT ( 'NONE',  ( 12.72792205982779734, -12.72792206288791128, -3.788324999819688177 ) ) ;
#19815 = FACE_OUTER_BOUND ( 'NONE', #13527, .T. ) ;
#19816 = EDGE_CURVE ( 'NONE', #12431, #13947, #19376, .T. ) ;
#19817 = ORIENTED_EDGE ( 'NONE', *, *, #18528, .F. ) ;
#19818 = ADVANCED_FACE ( 'NONE', ( #14827 ), #11631, .F. ) ;
#19819 = CARTESIAN_POINT ( 'NONE',  ( 0.000000000000000000, 43.56693332842786504, 48.57318520917521454 ) ) ;
#19820 = ORIENTED_EDGE ( 'NONE', *, *, #1580, .F. ) ;
#19821 = FACE_OUTER_BOUND ( 'NONE', #10757, .T. ) ;
#19822 = DIRECTION ( 'NONE',  ( -1.000000000000000000, -0.000000000000000000, -0.000000000000000000 ) ) ;
#19823 = CIRCLE ( 'NONE', #10005, 34.99999999999999289 ) ;
#19824 = ORIENTED_EDGE ( 'NONE', *, *, #6598, .F. ) ;
#19825 = ORIENTED_EDGE ( 'NONE', *, *, #9637, .T. ) ;
#19826 = CARTESIAN_POINT ( 'NONE',  ( 1.040949779275250179E-14, -85.00000000000000000, 19.00000000000000000 ) ) ;
#19827 = AXIS2_PLACEMENT_3D ( 'NONE', #7753, #7533, #10828 ) ;
#19828 = CARTESIAN_POINT ( 'NONE',  ( 9.999999999999998224, -44.69367065308607323, -56.44887778834792158 ) ) ;
#19829 = CARTESIAN_POINT ( 'NONE',  ( 0.000000000000000000, 0.000000000000000000, 0.000000000000000000 ) ) ;
#19830 = EDGE_CURVE ( 'NONE', #798, #3628, #18507, .T. ) ;
#19831 =( GEOMETRIC_REPRESENTATION_CONTEXT ( 3 ) GLOBAL_UNCERTAINTY_ASSIGNED_CONTEXT ( ( #8568 ) ) GLOBAL_UNIT_ASSIGNED_CONTEXT ( ( #8364, #3687, #6560 ) ) REPRESENTATION_CONTEXT ( 'NONE', 'WORKASPACE' ) );
#19832 = DIRECTION ( 'NONE',  ( -1.000000000000000000, 0.000000000000000000, -0.000000000000000000 ) ) ;
#19833 = AXIS2_PLACEMENT_3D ( 'NONE', #2339, #550, #18342 ) ;
#19834 = EDGE_CURVE ( 'NONE', #2130, #9768, #16472, .T. ) ;
#19835 = DIRECTION ( 'NONE',  ( 0.000000000000000000, 0.000000000000000000, 1.000000000000000000 ) ) ;
#19836 = DIRECTION ( 'NONE',  ( -0.7071067811865364705, 0.000000000000000000, 0.7071067811865584529 ) ) ;
#19837 = CARTESIAN_POINT ( 'NONE',  ( -31.74999999999995737, 0.000000000000000000, 0.000000000000000000 ) ) ;
#19838 = AXIS2_PLACEMENT_3D ( 'NONE', #19324, #6189, #15844 ) ;
#19839 = CIRCLE ( 'NONE', #15779, 65.24900000006525147 ) ;
#19840 = ORIENTED_EDGE ( 'NONE', *, *, #16065, .T. ) ;
#19841 = CARTESIAN_POINT ( 'NONE',  ( -2.870125741905213079, 6.929096494179683319, 3.693387500180313143 ) ) ;
#19842 = ORIENTED_EDGE ( 'NONE', *, *, #16847, .F. ) ;
#19843 = ADVANCED_FACE ( 'NONE', ( #8290 ), #193, .F. ) ;
#19844 = CARTESIAN_POINT ( 'NONE',  ( 19.99999999999999645, -28.84646472442415543, -58.52617768068463278 ) ) ;
#19845 = CARTESIAN_POINT ( 'NONE',  ( -18.69829135368511075, -10.63264222386861135, 76.60301815488043076 ) ) ;
#19846 = VERTEX_POINT ( 'NONE', #15993 ) ;
#19847 = DIRECTION ( 'NONE',  ( 0.000000000000000000, 1.224646799147353207E-16, 1.000000000000000000 ) ) ;
#19848 = ORIENTED_EDGE ( 'NONE', *, *, #673, .F. ) ;
#19849 = CARTESIAN_POINT ( 'NONE',  ( 19.99999999999999645, -59.31169354540756444, 27.19476070466835438 ) ) ;
#19850 = CARTESIAN_POINT ( 'NONE',  ( 5.000000000000000888, 0.000000000000000000, 0.000000000000000000 ) ) ;
#19851 = AXIS2_PLACEMENT_3D ( 'NONE', #746, #19822, #13683 ) ;
#19852 = VERTEX_POINT ( 'NONE', #6654 ) ;
#19853 = VECTOR ( 'NONE', #17214, 1000.000000000000000 ) ;
#19854 = AXIS2_PLACEMENT_3D ( 'NONE', #10264, #2208, #19995 ) ;
#19855 = EDGE_CURVE ( 'NONE', #10231, #18587, #3171, .T. ) ;
#19856 = CARTESIAN_POINT ( 'NONE',  ( 30.00000000000000000, -99.99999999999998579, 52.00000000000000000 ) ) ;
#19857 = CARTESIAN_POINT ( 'NONE',  ( -10.19618095414378445, -15.25966316918061239, -13.05620624981969513 ) ) ;
#19858 = CARTESIAN_POINT ( 'NONE',  ( 24.99999999999999645, -39.99999999999999289, 52.00000000000000000 ) ) ;
#19859 = ADVANCED_FACE ( 'NONE', ( #13228 ), #5160, .F. ) ;
#19860 = CIRCLE ( 'NONE', #10735, 72.00000000007199219 ) ;
#19861 = CARTESIAN_POINT ( 'NONE',  ( 0.000000000000000000, 1.178949249685212974, -2.042000000000001148 ) ) ;
#19862 = CARTESIAN_POINT ( 'NONE',  ( -6.330490858644140850, -9.474249097082498849, 0.8824535006474282239 ) ) ;
#19863 = VERTEX_POINT ( 'NONE', #16298 ) ;
#19864 = DIRECTION ( 'NONE',  ( 0.000000000000000000, 0.000000000000000000, 1.000000000000000000 ) ) ;
#19865 = ADVANCED_FACE ( 'NONE', ( #18104 ), #11222, .T. ) ;
#19866 = DIRECTION ( 'NONE',  ( -1.000000000000000000, 0.000000000000000000, -0.000000000000000000 ) ) ;
#19867 = VERTEX_POINT ( 'NONE', #8140 ) ;
#19868 = AXIS2_PLACEMENT_3D ( 'NONE', #20452, #4443, #15785 ) ;
#19869 = CARTESIAN_POINT ( 'NONE',  ( 19.99999999999999645, 0.000000000000000000, 0.000000000000000000 ) ) ;
#19870 = VERTEX_POINT ( 'NONE', #14614 ) ;
#19871 = AXIS2_PLACEMENT_3D ( 'NONE', #1046, #14291, #12493 ) ;
#19872 = CARTESIAN_POINT ( 'NONE',  ( -12.72792206288791128, -12.72792205982779912, -1.432074999819687333 ) ) ;
#19873 = DIRECTION ( 'NONE',  ( -1.000000000000000000, 0.000000000000000000, 0.000000000000000000 ) ) ;
#19874 = FACE_OUTER_BOUND ( 'NONE', #10197, .T. ) ;
#19875 = AXIS2_PLACEMENT_3D ( 'NONE', #4156, #2580, #20369 ) ;
#19876 = ORIENTED_EDGE ( 'NONE', *, *, #5169, .T. ) ;
#19877 = CIRCLE ( 'NONE', #4649, 5.000000000000004441 ) ;
#19878 = CARTESIAN_POINT ( 'NONE',  ( 50.00000000000000000, -160.0000000000000000, 0.000000000000000000 ) ) ;
#19879 = ORIENTED_EDGE ( 'NONE', *, *, #1481, .T. ) ;
#19880 = FILL_AREA_STYLE ('',( #5041 ) ) ;
#19881 = VECTOR ( 'NONE', #4322, 1000.000000000000000 ) ;
#19882 = EDGE_LOOP ( 'NONE', ( #14757, #15347, #2931, #8924 ) ) ;
#19883 = CARTESIAN_POINT ( 'NONE',  ( 0.000000000000000000, 0.000000000000000000, 129.0000000000000000 ) ) ;
#19884 = CIRCLE ( 'NONE', #9400, 10.00000000000000178 ) ;
#19885 = DIRECTION ( 'NONE',  ( 1.000000000000000000, -0.000000000000000000, -0.000000000000000000 ) ) ;
#19886 = ITEM_DEFINED_TRANSFORMATION ( 'NONE', 'NONE', #6255,  #12461 ) ;
#19887 = CARTESIAN_POINT ( 'NONE',  ( 5.663308650141532397, 13.67243654642775574, 13.97310441884154564 ) ) ;
#19889 = ORIENTED_EDGE ( 'NONE', *, *, #2248, .T. ) ;
#19888 = AXIS2_PLACEMENT_3D ( 'NONE', #14915, #18205, #16292 ) ;
#19890 = DIRECTION ( 'NONE',  ( 0.000000000000000000, 0.000000000000000000, 1.000000000000000000 ) ) ;
#19891 = CARTESIAN_POINT ( 'NONE',  ( 0.000000000000000000, 31.17893654894306721, -57.31758819669140337 ) ) ;
#19892 = CARTESIAN_POINT ( 'NONE',  ( -10.19618095047497874, 15.25966317163202746, 18.16410625018031411 ) ) ;
#19893 = DIRECTION ( 'NONE',  ( 0.000000000000000000, 0.000000000000000000, 1.000000000000000000 ) ) ;
#19894 = ORIENTED_EDGE ( 'NONE', *, *, #1806, .T. ) ;
#19895 = EDGE_CURVE ( 'NONE', #1438, #9255, #12510, .T. ) ;
#19896 = DIRECTION ( 'NONE',  ( -1.000000000000000000, 0.000000000000000000, 0.000000000000000000 ) ) ;
#19897 = VERTEX_POINT ( 'NONE', #11522 ) ;
#19898 = DIRECTION ( 'NONE',  ( 0.000000000000000000, 0.000000000000000000, -1.000000000000000000 ) ) ;
#19899 = ORIENTED_EDGE ( 'NONE', *, *, #5210, .T. ) ;
#19900 = CARTESIAN_POINT ( 'NONE',  ( 19.99999999999999645, 0.000000000000000000, 0.000000000000000000 ) ) ;
#19901 = CARTESIAN_POINT ( 'NONE',  ( -15.25966316918061416, 10.19618095414378445, -1.274956249819690024 ) ) ;
#19902 = VERTEX_POINT ( 'NONE', #3366 ) ;
#19903 = ORIENTED_EDGE ( 'NONE', *, *, #2295, .F. ) ;
#19904 = DIRECTION ( 'NONE',  ( 0.000000000000000000, -0.7812527682501556603, 0.6242147964454771714 ) ) ;
#19905 = FACE_OUTER_BOUND ( 'NONE', #17701, .T. ) ;
#19906 = FACE_OUTER_BOUND ( 'NONE', #17722, .T. ) ;
#19907 = CARTESIAN_POINT ( 'NONE',  ( -6.358192987158597376, 4.248408730893249441, -16.04020624981968624 ) ) ;
#19908 = CARTESIAN_POINT ( 'NONE',  ( 5.303300859536635770, 5.303300858261589923, -3.964424999819686324 ) ) ;
#19909 = AXIS2_PLACEMENT_3D ( 'NONE', #17296, #4362, #15589 ) ;
#19910 = CARTESIAN_POINT ( 'NONE',  ( 9.474249097082495297, -6.330490858644137298, -8.596516000286802850 ) ) ;
#19911 = FACE_OUTER_BOUND ( 'NONE', #5346, .T. ) ;
#19912 = DIRECTION ( 'NONE',  ( 0.000000000000000000, 0.000000000000000000, -1.000000000000000000 ) ) ;
#19913 = ORIENTED_EDGE ( 'NONE', *, *, #10375, .T. ) ;
#19914 = EDGE_CURVE ( 'NONE', #14529, #3964, #20527, .T. ) ;
#19915 = CARTESIAN_POINT ( 'NONE',  ( 21.45900938229203447, -1.326995226329880762, -84.99999999999998579 ) ) ;
#19916 = CARTESIAN_POINT ( 'NONE',  ( 16.62983158603122291, 6.888301780572502864, 3.869487500180311734 ) ) ;
#19917 = DIRECTION ( 'NONE',  ( 0.000000000000000000, 0.000000000000000000, 1.000000000000000000 ) ) ;
#19918 = ORIENTED_EDGE ( 'NONE', *, *, #6643, .F. ) ;
#19919 = DIRECTION ( 'NONE',  ( -1.000000000000000000, 0.000000000000000000, 0.000000000000000000 ) ) ;
#19920 = ORIENTED_EDGE ( 'NONE', *, *, #6864, .T. ) ;
#19921 = CYLINDRICAL_SURFACE ( 'NONE', #19999, 27.60000000002759890 ) ;
#19922 = DIRECTION ( 'NONE',  ( 0.000000000000000000, 0.8878852184023763305, -0.4600650377311499839 ) ) ;
#19923 = EDGE_LOOP ( 'NONE', ( #20210, #4578, #14641, #4670 ) ) ;
#19924 = ORIENTED_EDGE ( 'NONE', *, *, #272, .T. ) ;
#19925 = CARTESIAN_POINT ( 'NONE',  ( 5.200000000000002842, 0.000000000000000000, 2.500000000000000444 ) ) ;
#19926 = EDGE_CURVE ( 'NONE', #100, #1825, #11393, .T. ) ;
#19927 =( NAMED_UNIT ( * ) PLANE_ANGLE_UNIT ( ) SI_UNIT ( $, .RADIAN. ) );
#19928 = DIRECTION ( 'NONE',  ( -1.000000000000000000, -0.000000000000000000, 0.000000000000000000 ) ) ;
#19929 = DIRECTION ( 'NONE',  ( -1.000000000000000000, 0.000000000000000000, 0.000000000000000000 ) ) ;
#19930 = CARTESIAN_POINT ( 'NONE',  ( 4.248408729364575365, -6.358192988180014993, 1.846456250180310565 ) ) ;
#19931 = CARTESIAN_POINT ( 'NONE',  ( 19.99999999999999645, -15.58726123847893774, 62.93731870009398932 ) ) ;
#19932 = CARTESIAN_POINT ( 'NONE',  ( 19.99999999999999645, 65.23577793412344761, -1.313498510941930153 ) ) ;
#19933 = DIRECTION ( 'NONE',  ( -0.5000000000000037748, -0.8660254037844364872, 0.000000000000000000 ) ) ;
#19934 = LINE ( 'NONE', #7213, #3835 ) ;
#19935 = VERTEX_POINT ( 'NONE', #13754 ) ;
#19936 = CARTESIAN_POINT ( 'NONE',  ( 28.06187315134367566, -160.0000000000000000, -51.51416696573247833 ) ) ;
#19937 = EDGE_LOOP ( 'NONE', ( #6638, #6215, #9829, #5573 ) ) ;
#19938 = CARTESIAN_POINT ( 'NONE',  ( 18.00000000043041126, 3.580422610670019434, 2.259418750180313129 ) ) ;
#19939 = CARTESIAN_POINT ( 'NONE',  ( 4.119954785698633160, -21.10500016855061389, 70.74589478160184797 ) ) ;
#19940 = EDGE_LOOP ( 'NONE', ( #9011, #1497, #9097, #7045 ) ) ;
#19941 = CARTESIAN_POINT ( 'NONE',  ( -18.00000000000000000, 2.204364238465235428E-15, -90.00000000000000000 ) ) ;
#19942 = EDGE_LOOP ( 'NONE', ( #3579, #12656, #5458, #1344 ) ) ;
#19943 = CARTESIAN_POINT ( 'NONE',  ( 6.249999999999902300, -10.82531754730554496, -43.00000000000000000 ) ) ;
#19944 = CYLINDRICAL_SURFACE ( 'NONE', #15105, 65.24900000006525147 ) ;
#19945 = EDGE_LOOP ( 'NONE', ( #1867, #5187, #19606, #15580 ) ) ;
#19946 = ADVANCED_FACE ( 'NONE', ( #13445 ), #10359, .T. ) ;
#19947 = ADVANCED_FACE ( 'NONE', ( #15338 ), #11742, .F. ) ;
#19948 = DIRECTION ( 'NONE',  ( 0.000000000000000000, 0.000000000000000000, 1.000000000000000000 ) ) ;
#19949 = CARTESIAN_POINT ( 'NONE',  ( 6.888301784570727726, 16.62983158437509701, -8.638237499819693355 ) ) ;
#19950 = CARTESIAN_POINT ( 'NONE',  ( 52.00000000000000000, -99.99999999999998579, 5.000000000000000000 ) ) ;
#19951 = CIRCLE ( 'NONE', #12170, 10.85999999999999410 ) ;
#19952 = EDGE_CURVE ( 'NONE', #10498, #3661, #20187, .T. ) ;
#19953 = CARTESIAN_POINT ( 'NONE',  ( 0.000000000000000000, 0.000000000000000000, 126.0000000000000000 ) ) ;
#19954 = EDGE_CURVE ( 'NONE', #12290, #17620, #511, .T. ) ;
#19955 = CARTESIAN_POINT ( 'NONE',  ( -4.276731812588566939, 10.32494394809439875, 4.122297250647427802 ) ) ;
#19956 = ORIENTED_EDGE ( 'NONE', *, *, #5871, .T. ) ;
#19957 = DIRECTION ( 'NONE',  ( -1.000000000000000000, 1.202124453834178081E-10, 0.000000000000000000 ) ) ;
#19958 = ORIENTED_EDGE ( 'NONE', *, *, #12189, .F. ) ;
#19959 = CARTESIAN_POINT ( 'NONE',  ( -3.108800563652526439, -21.28778730843814415, -70.66877985699920828 ) ) ;
#19960 = ORIENTED_EDGE ( 'NONE', *, *, #12128, .T. ) ;
#19961 = CARTESIAN_POINT ( 'NONE',  ( 6.888301780572507305, -16.62983158603121936, -3.199262499819687022 ) ) ;
#19962 = CARTESIAN_POINT ( 'NONE',  ( 4.999999999999997335, 0.000000000000000000, 4.250000000000000000 ) ) ;
#19963 = CARTESIAN_POINT ( 'NONE',  ( -8.500000000000000000, 0.000000000000000000, -81.99999999999998579 ) ) ;
#19964 = ORIENTED_EDGE ( 'NONE', *, *, #8127, .T. ) ;
#19965 = EDGE_CURVE ( 'NONE', #510, #16131, #617, .T. ) ;
#19966 = ORIENTED_EDGE ( 'NONE', *, *, #11799, .F. ) ;
#19967 = DIRECTION ( 'NONE',  ( 0.000000000000000000, 0.000000000000000000, 1.000000000000000000 ) ) ;
#19968 = AXIS2_PLACEMENT_3D ( 'NONE', #5976, #9267, #12449 ) ;
#19969 = ORIENTED_EDGE ( 'NONE', *, *, #16069, .F. ) ;
#19970 = DIRECTION ( 'NONE',  ( 0.000000000000000000, 0.000000000000000000, 1.000000000000000000 ) ) ;
#19971 = EDGE_CURVE ( 'NONE', #6180, #10026, #9714, .T. ) ;
#19972 = ORIENTED_EDGE ( 'NONE', *, *, #15706, .F. ) ;
#19973 = DIRECTION ( 'NONE',  ( -1.000000000000000000, -0.000000000000000000, 0.000000000000000000 ) ) ;
#19974 = EDGE_CURVE ( 'NONE', #15733, #9763, #17184, .T. ) ;
#19975 = CARTESIAN_POINT ( 'NONE',  ( 30.00000000000000000, -50.00000000000000000, 66.88656633939929463 ) ) ;
#19976 = CARTESIAN_POINT ( 'NONE',  ( -14.79893867722910628, 2.943691928843437111, 20.74732316884154670 ) ) ;
#19977 = ORIENTED_EDGE ( 'NONE', *, *, #1328, .T. ) ;
#19978 = CIRCLE ( 'NONE', #10865, 72.00000000007199219 ) ;
#19979 = DIRECTION ( 'NONE',  ( -1.000000000000000000, -0.000000000000000000, 0.000000000000000000 ) ) ;
#19980 = CARTESIAN_POINT ( 'NONE',  ( -13.12108515385492247, -17.04513403132573046, 78.38820092699481279 ) ) ;
#19981 = CARTESIAN_POINT ( 'NONE',  ( 8.382925368423265411, -12.54593441764187034, -16.68013566848092566 ) ) ;
#19982 = DIRECTION ( 'NONE',  ( 0.000000000000000000, 0.000000000000000000, 1.000000000000000000 ) ) ;
#19983 = AXIS2_PLACEMENT_3D ( 'NONE', #19543, #8405, #3424 ) ;
#19984 = EDGE_CURVE ( 'NONE', #8060, #8274, #2957, .T. ) ;
#19985 = ORIENTED_EDGE ( 'NONE', *, *, #5468, .F. ) ;
#19986 = CARTESIAN_POINT ( 'NONE',  ( 30.06717155927020713, -106.8759708378635054, 77.91277504389037745 ) ) ;
#19987 = CARTESIAN_POINT ( 'NONE',  ( 42.29298993630181513, -123.8503867192492578, -81.55043513968610114 ) ) ;
#19988 = ORIENTED_EDGE ( 'NONE', *, *, #4192, .T. ) ;
#19989 = CARTESIAN_POINT ( 'NONE',  ( 4.248408729364579806, -6.358192988180021210, 8.111356250180314476 ) ) ;
#19990 = ORIENTED_EDGE ( 'NONE', *, *, #19805, .F. ) ;
#19991 = FACE_OUTER_BOUND ( 'NONE', #6554, .T. ) ;
#19992 = CARTESIAN_POINT ( 'NONE',  ( 12.72792206288790773, 12.72792205982779912, 1.375825000180311175 ) ) ;
#19993 = ORIENTED_EDGE ( 'NONE', *, *, #1587, .T. ) ;
#19994 = ORIENTED_EDGE ( 'NONE', *, *, #5685, .T. ) ;
#19995 = DIRECTION ( 'NONE',  ( 0.000000000000000000, 0.000000000000000000, 1.000000000000000000 ) ) ;
#19996 = AXIS2_PLACEMENT_3D ( 'NONE', #13181, #5018, #6702 ) ;
#19997 = CARTESIAN_POINT ( 'NONE',  ( -24.99999999999999289, -170.8299878242309546, 15.48896927112552824 ) ) ;
#19998 = DIRECTION ( 'NONE',  ( -1.000000000000000000, -0.000000000000000000, 0.000000000000000000 ) ) ;
#19999 = AXIS2_PLACEMENT_3D ( 'NONE', #5609, #18654, #8691 ) ;
#20000 = CARTESIAN_POINT ( 'NONE',  ( 1.491842756249030399, 7.499999999820669672, -14.27301874981969121 ) ) ;
#20001 = PRODUCT_DEFINITION_CONTEXT ( 'detailed design', #11155, 'design' ) ;
#20002 = ADVANCED_FACE ( 'NONE', ( #15227 ), #395, .F. ) ;
#20003 = DIRECTION ( 'NONE',  ( 0.000000000000000000, 0.000000000000000000, 1.000000000000000000 ) ) ;
#20004 = CARTESIAN_POINT ( 'NONE',  ( -9.015947181032835626E-10, -7.500000000000007994, -9.855049999819689432 ) ) ;
#20005 = CARTESIAN_POINT ( 'NONE',  ( -7.902369976724391343, 7.902369978624323110, -22.43948475028680889 ) ) ;
#20006 = FACE_OUTER_BOUND ( 'NONE', #4258, .T. ) ;
#20007 = CIRCLE ( 'NONE', #13954, 72.00000000007199219 ) ;
#20008 = AXIS2_PLACEMENT_3D ( 'NONE', #4684, #14544, #14636 ) ;
#20009 = EDGE_LOOP ( 'NONE', ( #7139, #15513, #8590, #17501 ) ) ;
#20010 = DIRECTION ( 'NONE',  ( -1.000000000000000000, 0.000000000000000000, 0.000000000000000000 ) ) ;
#20011 = CARTESIAN_POINT ( 'NONE',  ( -16.62983158437510056, 6.888301784570729502, 0.3351125001803123560 ) ) ;
#20012 = CARTESIAN_POINT ( 'NONE',  ( 0.000000000000000000, -38.69327817041740047, -52.53819777490674880 ) ) ;
#20013 = AXIS2_PLACEMENT_3D ( 'NONE', #14424, #5251, #17912 ) ;
#20014 = VERTEX_POINT ( 'NONE', #19787 ) ;
#20015 = DIRECTION ( 'NONE',  ( 1.000000000000000000, 0.000000000000000000, 0.000000000000000000 ) ) ;
#20016 = EDGE_LOOP ( 'NONE', ( #4242, #1985 ) ) ;
#20017 = DIRECTION ( 'NONE',  ( 0.000000000000000000, -0.000000000000000000, -1.000000000000000000 ) ) ;
#20018 = CARTESIAN_POINT ( 'NONE',  ( 38.45380490109781135, -18.24950758230019332, -72.03149080720356778 ) ) ;
#20019 = ORIENTED_EDGE ( 'NONE', *, *, #7645, .F. ) ;
#20020 = AXIS2_PLACEMENT_3D ( 'NONE', #19858, #10003, #3051 ) ;
#20021 = ORIENTED_EDGE ( 'NONE', *, *, #17513, .T. ) ;
#20022 = FACE_OUTER_BOUND ( 'NONE', #9674, .T. ) ;
#20023 =( LENGTH_UNIT ( ) NAMED_UNIT ( * ) SI_UNIT ( .MILLI., .METRE. ) );
#20024 = FACE_OUTER_BOUND ( 'NONE', #18391, .T. ) ;
#20025 = CIRCLE ( 'NONE', #10573, 2.650000000000000355 ) ;
#20026 = AXIS2_PLACEMENT_3D ( 'NONE', #5706, #965, #2854 ) ;
#20027 = EDGE_CURVE ( 'NONE', #834, #15340, #4300, .T. ) ;
#20028 = CARTESIAN_POINT ( 'NONE',  ( 6.249999999999902300, -10.82531754730554496, 43.00000000000000000 ) ) ;
#20029 = CARTESIAN_POINT ( 'NONE',  ( -6.929096494179677101, -2.870125741905209527, -14.35276249981968988 ) ) ;
#20030 = CARTESIAN_POINT ( 'NONE',  ( 30.00000000000000000, -99.99999999999998579, -52.00000000000000000 ) ) ;
#20031 = CARTESIAN_POINT ( 'NONE',  ( 0.2500000000000002220, 0.000000000000000000, 4.000000000000000000 ) ) ;
#20032 = LINE ( 'NONE', #5727, #11198 ) ;
#20033 = CARTESIAN_POINT ( 'NONE',  ( 19.99999999999999645, 23.08379033237351052, 61.02926039941442582 ) ) ;
#20034 = VERTEX_POINT ( 'NONE', #16715 ) ;
#20035 = CARTESIAN_POINT ( 'NONE',  ( 7.500000000000007105, 4.207617034055637320E-15, 6.638700000002313750 ) ) ;
#20036 = VERTEX_POINT ( 'NONE', #13648 ) ;
#20037 = CARTESIAN_POINT ( 'NONE',  ( 15.25966317163202746, 10.19618095047498407, 11.09535625018031446 ) ) ;
#20038 = CARTESIAN_POINT ( 'NONE',  ( -19.43057967899845551, -9.208910241125163765, 77.65734690581830080 ) ) ;
#20039 = AXIS2_PLACEMENT_3D ( 'NONE', #3664, #5145, #13017 ) ;
#20040 = EDGE_LOOP ( 'NONE', ( #8192, #11983, #10572, #4350 ) ) ;
#20041 = AXIS2_PLACEMENT_3D ( 'NONE', #7829, #16104, #3272 ) ;
#20042 = DIRECTION ( 'NONE',  ( 0.000000000000000000, 0.000000000000000000, 1.000000000000000000 ) ) ;
#20043 = ORIENTED_EDGE ( 'NONE', *, *, #11853, .F. ) ;
#20044 = CARTESIAN_POINT ( 'NONE',  ( 19.99999999999999645, 29.55812890831981932, 65.65300461859696668 ) ) ;
#20045 = DIRECTION ( 'NONE',  ( 0.000000000000000000, 0.7308359642781206977, 0.6825531432186578984 ) ) ;
#20046 = VECTOR ( 'NONE', #1994, 999.9999999999998863 ) ;
#20047 = CIRCLE ( 'NONE', #10927, 27.60000000002759890 ) ;
#20048 = ORIENTED_EDGE ( 'NONE', *, *, #7956, .T. ) ;
#20049 = DIRECTION ( 'NONE',  ( 0.000000000000000000, 0.000000000000000000, 1.000000000000000000 ) ) ;
#20050 = CIRCLE ( 'NONE', #10930, 7.500000000000000000 ) ;
#20051 = CARTESIAN_POINT ( 'NONE',  ( -30.00000000000000000, -40.00000000000000000, -130.0000000000000000 ) ) ;
#20052 = CARTESIAN_POINT ( 'NONE',  ( 12.72792206288790773, 12.72792205982779912, -17.47417499981969513 ) ) ;
#20053 = CARTESIAN_POINT ( 'NONE',  ( 30.00000000000000000, -50.00000000000000000, -66.88656633939928042 ) ) ;
#20054 = CARTESIAN_POINT ( 'NONE',  ( 6.249999999999902300, -10.82531754730554496, 46.00000000000000711 ) ) ;
#20055 = CARTESIAN_POINT ( 'NONE',  ( 2.222972768810839383, -11.17563879758428769, -0.2956714993525706436 ) ) ;
#20056 = CIRCLE ( 'NONE', #6199, 21.50000000000000000 ) ;
#20058 = ORIENTED_EDGE ( 'NONE', *, *, #19713, .F. ) ;
#20057 = AXIS2_PLACEMENT_3D ( 'NONE', #3936, #2153, #18259 ) ;
#20059 = DIRECTION ( 'NONE',  ( 0.000000000000000000, 0.000000000000000000, 1.000000000000000000 ) ) ;
#20060 = CARTESIAN_POINT ( 'NONE',  ( 18.13963350654227469, -26.35784117651622793, -130.0000000000000000 ) ) ;
#20061 = VERTEX_POINT ( 'NONE', #10569 ) ;
#20062 = CARTESIAN_POINT ( 'NONE',  ( 19.54001732319277096, -8.991134644608420601, -77.82005195698282307 ) ) ;
#20063 = ADVANCED_FACE ( 'NONE', ( #17465 ), #20303, .T. ) ;
#20064 = ORIENTED_EDGE ( 'NONE', *, *, #20904, .F. ) ;
#20065 = EDGE_CURVE ( 'NONE', #10032, #20507, #18519, .T. ) ;
#20066 = CARTESIAN_POINT ( 'NONE',  ( 17.99999999956958163, -3.580422614997676334, 4.753081250180313688 ) ) ;
#20067 = CARTESIAN_POINT ( 'NONE',  ( 19.99999999999999645, -55.05624179292004072, 35.01774179823764399 ) ) ;
#20068 = FACE_OUTER_BOUND ( 'NONE', #9988, .T. ) ;
#20069 = AXIS2_PLACEMENT_3D ( 'NONE', #14833, #13235, #11341 ) ;
#20070 = ORIENTED_EDGE ( 'NONE', *, *, #3343, .F. ) ;
#20071 = FACE_OUTER_BOUND ( 'NONE', #16177, .T. ) ;
#20072 = EDGE_LOOP ( 'NONE', ( #17311, #6464, #20644, #16353 ) ) ;
#20073 = CARTESIAN_POINT ( 'NONE',  ( -4.000000000000000000, -2.309401076758525573, -5.599999999999999645 ) ) ;
#20074 = EDGE_CURVE ( 'NONE', #1607, #14245, #17250, .T. ) ;
#20075 = VERTEX_POINT ( 'NONE', #4416 ) ;
#20076 = CIRCLE ( 'NONE', #5535, 2.649999999999992806 ) ;
#20077 = DIRECTION ( 'NONE',  ( 0.000000000000000000, 0.000000000000000000, -1.000000000000000000 ) ) ;
#20078 = CIRCLE ( 'NONE', #12318, 8.999999999999994671 ) ;
#20079 = ORIENTED_EDGE ( 'NONE', *, *, #1368, .F. ) ;
#20080 = DIRECTION ( 'NONE',  ( -0.000000000000000000, 1.000000000000000000, 1.224646799147353207E-16 ) ) ;
#20081 = CARTESIAN_POINT ( 'NONE',  ( 0.000000000000000000, -63.85430960833482317, -11.25592921604904539 ) ) ;
#20082 = CARTESIAN_POINT ( 'NONE',  ( 5.663308646854342321, -13.67243654778935635, 17.50747941884155168 ) ) ;
#20083 = CIRCLE ( 'NONE', #13326, 72.00000000007199219 ) ;
#20084 = EDGE_CURVE ( 'NONE', #14491, #20014, #1362, .T. ) ;
#20085 = ORIENTED_EDGE ( 'NONE', *, *, #6486, .F. ) ;
#20086 = DIRECTION ( 'NONE',  ( 1.000000000000000000, 0.000000000000000000, 0.000000000000000000 ) ) ;
#20087 = AXIS2_PLACEMENT_3D ( 'NONE', #20028, #4026, #16962 ) ;
#20088 = CARTESIAN_POINT ( 'NONE',  ( -14.15758254428918228, -16.19451531421082535, 78.90478163254508104 ) ) ;
#20089 = ADVANCED_FACE ( 'NONE', ( #2720 ), #9188, .T. ) ;
#20090 = CARTESIAN_POINT ( 'NONE',  ( 2.163825119083639120E-09, 17.99999999999999645, 19.04770000018030984 ) ) ;
#20091 = VECTOR ( 'NONE', #13082, 1000.000000000000000 ) ;
#20092 = ADVANCED_FACE ( 'NONE', ( #18737 ), #2522, .T. ) ;
#20093 = CARTESIAN_POINT ( 'NONE',  ( -2.000000000000022649, -3.464101615137742396, 0.000000000000000000 ) ) ;
#20094 = EDGE_LOOP ( 'NONE', ( #14623, #17843, #1976, #1361 ) ) ;
#20095 = EDGE_CURVE ( 'NONE', #349, #18213, #8022, .T. ) ;
#20096 = DIRECTION ( 'NONE',  ( -1.000000000000000000, 0.000000000000000000, 0.000000000000000000 ) ) ;
#20097 = DIRECTION ( 'NONE',  ( -1.000000000000000000, 0.000000000000000000, 0.000000000000000000 ) ) ;
#20098 = AXIS2_PLACEMENT_3D ( 'NONE', #16440, #19417, #6787 ) ;
#20099 = ORIENTED_EDGE ( 'NONE', *, *, #19260, .F. ) ;
#20100 = CARTESIAN_POINT ( 'NONE',  ( 3.105127573534534502, -22.79270295337239105, -75.46210090792683900 ) ) ;
#20101 = EDGE_LOOP ( 'NONE', ( #1453, #15749 ) ) ;
#20102 = CARTESIAN_POINT ( 'NONE',  ( -10.00000000000000000, 0.000000000000000000, 0.000000000000000000 ) ) ;
#20103 = CARTESIAN_POINT ( 'NONE',  ( 10.19618095047497697, -15.25966317163202923, 4.026606250180309488 ) ) ;
#20104 = ORIENTED_EDGE ( 'NONE', *, *, #10266, .T. ) ;
#20105 = EDGE_LOOP ( 'NONE', ( #14829, #5040 ) ) ;
#20106 = CYLINDRICAL_SURFACE ( 'NONE', #17499, 5.000000000000004441 ) ;
#20107 = AXIS2_PLACEMENT_3D ( 'NONE', #11462, #19298, #6375 ) ;
#20108 = EDGE_CURVE ( 'NONE', #2027, #16324, #1262, .T. ) ;
#20109 = CARTESIAN_POINT ( 'NONE',  ( 0.000000000000000000, 0.000000000000000000, -0.3080913168122707546 ) ) ;
#20110 = CARTESIAN_POINT ( 'NONE',  ( 8.899999999999895550, -10.82531754730554496, 129.0000000000000000 ) ) ;
#20111 = EDGE_CURVE ( 'NONE', #13834, #10203, #16491, .T. ) ;
#20112 = CARTESIAN_POINT ( 'NONE',  ( -12.72792205982780089, 12.72792206288791128, 19.77417500018031049 ) ) ;
#20113 = EDGE_CURVE ( 'NONE', #2104, #12463, #10685, .T. ) ;
#20114 = EDGE_CURVE ( 'NONE', #8758, #5518, #3616, .T. ) ;
#20115 = DIRECTION ( 'NONE',  ( -0.000000000000000000, -0.000000000000000000, -1.000000000000000000 ) ) ;
#20116 = CARTESIAN_POINT ( 'NONE',  ( 7.499999999820668783, -1.491842756249033508, 6.933231250180315719 ) ) ;
#20117 = CARTESIAN_POINT ( 'NONE',  ( 0.000000000000000000, 5.762283366691162811, 64.99406197038673838 ) ) ;
#20118 = CARTESIAN_POINT ( 'NONE',  ( -4.276731815070945686, -10.32494394706615637, -6.534797250286804804 ) ) ;
#20119 = EDGE_CURVE ( 'NONE', #10244, #13762, #14126, .T. ) ;
#20120 = DIRECTION ( 'NONE',  ( -1.000000000000000000, -0.000000000000000000, -0.000000000000000000 ) ) ;
#20121 = VECTOR ( 'NONE', #6205, 1000.000000000000000 ) ;
#20122 = ORIENTED_EDGE ( 'NONE', *, *, #12990, .F. ) ;
#20123 = CARTESIAN_POINT ( 'NONE',  ( 2.000000000000027089, 3.464101615137739731, -5.600000000000000533 ) ) ;
#20124 = CARTESIAN_POINT ( 'NONE',  ( -16.62983158603122291, -6.888301780572501087, -10.26801249981968844 ) ) ;
#20125 = DIRECTION ( 'NONE',  ( -1.000000000000000000, 0.000000000000000000, 0.000000000000000000 ) ) ;
#20126 = ORIENTED_EDGE ( 'NONE', *, *, #14554, .F. ) ;
#20127 = DIRECTION ( 'NONE',  ( -1.000000000000000000, 0.000000000000000000, 0.000000000000000000 ) ) ;
#20128 = ORIENTED_EDGE ( 'NONE', *, *, #9370, .F. ) ;
#20129 = FACE_OUTER_BOUND ( 'NONE', #19461, .T. ) ;
#20130 = CARTESIAN_POINT ( 'NONE',  ( -39.99999999999999289, -30.00000000000000000, -130.0000000000000000 ) ) ;
#20131 = ORIENTED_EDGE ( 'NONE', *, *, #16960, .T. ) ;
#20132 = ORIENTED_EDGE ( 'NONE', *, *, #3890, .T. ) ;
#20133 = CARTESIAN_POINT ( 'NONE',  ( 19.99999999999999645, 0.000000000000000000, 0.000000000000000000 ) ) ;
#20134 = CARTESIAN_POINT ( 'NONE',  ( 19.99999999999999645, -55.05624179291956466, -35.01774179823839717 ) ) ;
#20135 = CIRCLE ( 'NONE', #863, 65.24900000006525147 ) ;
#20136 = CYLINDRICAL_SURFACE ( 'NONE', #10973, 5.000000000000004441 ) ;
#20137 = CARTESIAN_POINT ( 'NONE',  ( 9.015937996181834148E-10, 7.500000000000000888, -1.982449999819689612 ) ) ;
#20138 = CARTESIAN_POINT ( 'NONE',  ( 0.000000000000000000, 0.000000000000000000, -90.00000000000000000 ) ) ;
#20139 = CARTESIAN_POINT ( 'NONE',  ( 4.000000000000002665, 1.557668341133517043, -5.440303434304241570 ) ) ;
#20140 = DIRECTION ( 'NONE',  ( 0.000000000000000000, 0.4999999999999990008, -0.8660254037844391517 ) ) ;
#20141 = ORIENTED_EDGE ( 'NONE', *, *, #9467, .F. ) ;
#20142 = CARTESIAN_POINT ( 'NONE',  ( -4.248408729364580694, 6.358192988180020322, 3.398856250180316341 ) ) ;
#20143 = AXIS2_PLACEMENT_3D ( 'NONE', #2470, #8933, #20267 ) ;
#20144 = ORIENTED_EDGE ( 'NONE', *, *, #15582, .F. ) ;
#20145 = CARTESIAN_POINT ( 'NONE',  ( 6.888301780572507305, -16.62983158603121936, 4.321137500180313396 ) ) ;
#20146 = CARTESIAN_POINT ( 'NONE',  ( -21.39626923676110692, -2.341574137301850822, 83.84978971573227113 ) ) ;
#20147 = ORIENTED_EDGE ( 'NONE', *, *, #3026, .F. ) ;
#20148 = ADVANCED_FACE ( 'NONE', ( #4525 ), #10789, .T. ) ;
#20149 = DIRECTION ( 'NONE',  ( -0.000000000000000000, -3.469446951953614682E-16, -1.000000000000000000 ) ) ;
#20150 = ORIENTED_EDGE ( 'NONE', *, *, #17562, .T. ) ;
#20151 = CIRCLE ( 'NONE', #11030, 2.649999999999999467 ) ;
#20152 = PRODUCT_DEFINITION_SHAPE ( 'NONE', 'NONE',  #20967 ) ;
#20153 = DIRECTION ( 'NONE',  ( -1.000000000000000000, 0.000000000000000000, 0.000000000000000000 ) ) ;
#20154 = DIRECTION ( 'NONE',  ( -1.000000000000000000, -0.000000000000000000, -0.000000000000000000 ) ) ;
#20155 = EDGE_CURVE ( 'NONE', #14998, #15789, #10989, .T. ) ;
#20156 = ORIENTED_EDGE ( 'NONE', *, *, #820, .F. ) ;
#20157 = DIRECTION ( 'NONE',  ( -1.000000000000000000, 0.000000000000000000, 0.000000000000000000 ) ) ;
#20158 = CARTESIAN_POINT ( 'NONE',  ( 0.000000000000000000, 0.000000000000000000, 0.000000000000000000 ) ) ;
#20159 = CARTESIAN_POINT ( 'NONE',  ( 17.99999999999999645, -2.163824016901520184E-09, -16.29604999981969371 ) ) ;
#20160 = DIRECTION ( 'NONE',  ( 0.000000000000000000, 0.000000000000000000, -1.000000000000000000 ) ) ;
#20161 = AXIS2_PLACEMENT_3D ( 'NONE', #15877, #1164, #9310 ) ;
#20162 = CIRCLE ( 'NONE', #2588, 2.649999999999999467 ) ;
#20163 = CARTESIAN_POINT ( 'NONE',  ( 5.000000000000000888, 0.000000000000000000, 0.000000000000000000 ) ) ;
#20164 = CARTESIAN_POINT ( 'NONE',  ( -4.276731815070949239, -10.32494394706616347, -18.26207774935257078 ) ) ;
#20165 = EDGE_LOOP ( 'NONE', ( #7646, #18106 ) ) ;
#20166 = CIRCLE ( 'NONE', #16786, 10.00000000000000178 ) ;
#20167 = VECTOR ( 'NONE', #13105, 1000.000000000000114 ) ;
#20168 = SURFACE_STYLE_FILL_AREA ( #7236 ) ;
#20169 = CARTESIAN_POINT ( 'NONE',  ( 19.99999999999999645, 55.05624179291979914, 35.01774179823801347 ) ) ;
#20170 = ORIENTED_EDGE ( 'NONE', *, *, #8053, .F. ) ;
#20171 = EDGE_CURVE ( 'NONE', #1772, #3060, #936, .T. ) ;
#20172 = CARTESIAN_POINT ( 'NONE',  ( 1.457308041610593241, -21.46427008073574783, -70.59507481315787913 ) ) ;
#20173 = ORIENTED_EDGE ( 'NONE', *, *, #3395, .T. ) ;
#20174 = CARTESIAN_POINT ( 'NONE',  ( 10.19618095047497874, -15.25966317163203279, 5.931206250180311557 ) ) ;
#20175 = VECTOR ( 'NONE', #17423, 1000.000000000000000 ) ;
#20176 = DIRECTION ( 'NONE',  ( 0.000000000000000000, 0.7308359642781208088, 0.6825531432186576763 ) ) ;
#20177 = DIRECTION ( 'NONE',  ( -0.000000000000000000, -0.000000000000000000, -1.000000000000000000 ) ) ;
#20178 = ORIENTED_EDGE ( 'NONE', *, *, #2330, .T. ) ;
#20179 = DIRECTION ( 'NONE',  ( 1.000000000000000000, 0.000000000000000000, -0.000000000000000000 ) ) ;
#20180 = CIRCLE ( 'NONE', #1601, 20.00000000000000000 ) ;
#20181 = ORIENTED_EDGE ( 'NONE', *, *, #12317, .F. ) ;
#20182 = CARTESIAN_POINT ( 'NONE',  ( -5.303300858261589035, 5.303300859536635770, 12.52932500018031448 ) ) ;
#20183 = EDGE_CURVE ( 'NONE', #11488, #14272, #12425, .T. ) ;
#20184 = AXIS2_PLACEMENT_3D ( 'NONE', #15237, #7177, #3996 ) ;
#20185 = ORIENTED_EDGE ( 'NONE', *, *, #20628, .T. ) ;
#20186 = DIRECTION ( 'NONE',  ( -1.000000000000000000, 0.000000000000000000, -0.000000000000000000 ) ) ;
#20187 = CIRCLE ( 'NONE', #4629, 65.24900000006526568 ) ;
#20188 = AXIS2_PLACEMENT_3D ( 'NONE', #13838, #15107, #16797 ) ;
#20189 = CARTESIAN_POINT ( 'NONE',  ( 0.000000000000000000, -36.59093685910671212, 62.00889726308019334 ) ) ;
#20190 = EDGE_CURVE ( 'NONE', #1625, #17634, #15480, .T. ) ;
#20191 = AXIS2_PLACEMENT_3D ( 'NONE', #20657, #11129, #7415 ) ;
#20192 = CYLINDRICAL_SURFACE ( 'NONE', #767, 75.00000000000000000 ) ;
#20193 = ITEM_DEFINED_TRANSFORMATION ( 'NONE', 'NONE', #3535,  #12461 ) ;
#20194 = CARTESIAN_POINT ( 'NONE',  ( -5.663308646854337880, 13.67243654778935991, 3.369979418841543506 ) ) ;
#20195 = ORIENTED_EDGE ( 'NONE', *, *, #4677, .F. ) ;
#20196 = AXIS2_PLACEMENT_3D ( 'NONE', #16697, #19973, #11923 ) ;
#20197 = DIRECTION ( 'NONE',  ( -0.000000000000000000, -0.000000000000000000, -1.000000000000000000 ) ) ;
#20198 = EDGE_CURVE ( 'NONE', #9451, #18686, #13790, .T. ) ;
#20199 = EDGE_CURVE ( 'NONE', #5038, #19685, #19575, .T. ) ;
#20200 = DIRECTION ( 'NONE',  ( -1.000000000000000000, -0.000000000000000000, 0.000000000000000000 ) ) ;
#20201 = AXIS2_PLACEMENT_3D ( 'NONE', #7380, #12699, #13856 ) ;
#20202 = CARTESIAN_POINT ( 'NONE',  ( -5.663308650141535949, -13.67243654642774686, -24.63247941848092637 ) ) ;
#20203 = FACE_OUTER_BOUND ( 'NONE', #1948, .T. ) ;
#20204 = ORIENTED_EDGE ( 'NONE', *, *, #19895, .F. ) ;
#20205 = CARTESIAN_POINT ( 'NONE',  ( -10.00000000000000000, 0.000000000000000000, 0.000000000000000000 ) ) ;
#20206 = CARTESIAN_POINT ( 'NONE',  ( 30.00000000000000000, -99.99999999999998579, 49.90000000000000568 ) ) ;
#20207 = CIRCLE ( 'NONE', #16161, 65.24900000006526568 ) ;
#20208 = ORIENTED_EDGE ( 'NONE', *, *, #8181, .T. ) ;
#20209 = CARTESIAN_POINT ( 'NONE',  ( 30.00000000000000000, -85.00000000000000000, -1.040949779275250179E-14 ) ) ;
#20210 = ORIENTED_EDGE ( 'NONE', *, *, #11371, .F. ) ;
#20211 = CARTESIAN_POINT ( 'NONE',  ( -10.00000000000000000, 0.000000000000000000, 0.000000000000000000 ) ) ;
#20212 = CARTESIAN_POINT ( 'NONE',  ( -3.580422610670017658, 18.00000000043040771, 9.328168750180312330 ) ) ;
#20213 = CIRCLE ( 'NONE', #12455, 4.000000000000000000 ) ;
#20214 = ORIENTED_EDGE ( 'NONE', *, *, #5905, .F. ) ;
#20215 = VERTEX_POINT ( 'NONE', #1766 ) ;
#20216 = CARTESIAN_POINT ( 'NONE',  ( 48.35276434571220250, -3.649167310370807105, -90.00000000000000000 ) ) ;
#20217 = EDGE_CURVE ( 'NONE', #5544, #16141, #4648, .T. ) ;
#20218 = AXIS2_PLACEMENT_3D ( 'NONE', #18867, #4340, #10705 ) ;
#20219 = FACE_OUTER_BOUND ( 'NONE', #12183, .T. ) ;
#20220 = EDGE_CURVE ( 'NONE', #12782, #15733, #8220, .T. ) ;
#20221 = CARTESIAN_POINT ( 'NONE',  ( 19.99999999999999645, -27.62776854598816101, -58.65812137499030854 ) ) ;
#20222 = CARTESIAN_POINT ( 'NONE',  ( 19.99999999999999645, -63.85430960833482317, -11.25592921604904539 ) ) ;
#20223 = CARTESIAN_POINT ( 'NONE',  ( -15.25966317163203456, -10.19618095047498230, 17.71245625018031333 ) ) ;
#20224 = PRODUCT_DEFINITION_CONTEXT ( 'detailed design', #12920, 'design' ) ;
#20226 = EDGE_CURVE ( 'NONE', #11557, #16083, #16821, .T. ) ;
#20225 = DIRECTION ( 'NONE',  ( 0.000000000000000000, 0.000000000000000000, 1.000000000000000000 ) ) ;
#20227 = CARTESIAN_POINT ( 'NONE',  ( 6.929096493489630859, -2.870125743571144472, -2.197237499819686857 ) ) ;
#20228 = EDGE_CURVE ( 'NONE', #11622, #7171, #20837, .T. ) ;
#20229 = DIRECTION ( 'NONE',  ( -1.000000000000000000, -0.000000000000000000, -0.000000000000000000 ) ) ;
#20230 = CARTESIAN_POINT ( 'NONE',  ( -2.222972771497743416, -11.17563879704981566, -6.829328500286805159 ) ) ;
#20231 = CIRCLE ( 'NONE', #19504, 27.60000000002760245 ) ;
#20232 = FACE_OUTER_BOUND ( 'NONE', #16976, .T. ) ;
#20233 = ORIENTED_EDGE ( 'NONE', *, *, #17632, .T. ) ;
#20234 = CYLINDRICAL_SURFACE ( 'NONE', #76, 7.500000000000000000 ) ;
#20235 = CARTESIAN_POINT ( 'NONE',  ( 3.580422614997668340, 17.99999999956958519, 2.396831250180312622 ) ) ;
#20236 = CARTESIAN_POINT ( 'NONE',  ( 50.00000000000000000, -42.57363661491096707, 121.3828884801879155 ) ) ;
#20237 = EDGE_CURVE ( 'NONE', #232, #19414, #97, .T. ) ;
#20238 = ORIENTED_EDGE ( 'NONE', *, *, #565, .F. ) ;
#20239 = EDGE_CURVE ( 'NONE', #1536, #18341, #169, .T. ) ;
#20240 = CYLINDRICAL_SURFACE ( 'NONE', #11570, 72.00000000007199219 ) ;
#20241 = VERTEX_POINT ( 'NONE', #11411 ) ;
#20242 = CYLINDRICAL_SURFACE ( 'NONE', #8168, 27.60000000002759890 ) ;
#20243 = DIRECTION ( 'NONE',  ( -0.000000000000000000, 0.000000000000000000, 1.000000000000000000 ) ) ;
#20244 = ORIENTED_EDGE ( 'NONE', *, *, #978, .T. ) ;
#20245 = VERTEX_POINT ( 'NONE', #13109 ) ;
#20246 = CARTESIAN_POINT ( 'NONE',  ( 50.00000000000000000, -3.649167310370807105, -90.00000000000000000 ) ) ;
#20247 = EDGE_CURVE ( 'NONE', #8902, #18188, #12904, .T. ) ;
#20248 = FILL_AREA_STYLE ('',( #5720 ) ) ;
#20249 = CARTESIAN_POINT ( 'NONE',  ( 14.50000000000000888, -85.00000000000000000, 5.000000000000000000 ) ) ;
#20250 = DIRECTION ( 'NONE',  ( -1.000000000000000000, -0.000000000000000000, -0.000000000000000000 ) ) ;
#20251 = CARTESIAN_POINT ( 'NONE',  ( 1.491842754445842134, -7.500000000179339210, -6.989481249819688102 ) ) ;
#20252 = DIRECTION ( 'NONE',  ( -1.000000000000000000, -0.000000000000000000, 0.000000000000000000 ) ) ;
#20253 = DIRECTION ( 'NONE',  ( -0.000000000000000000, -0.000000000000000000, 1.000000000000000000 ) ) ;
#20254 = LINE ( 'NONE', #6154, #13063 ) ;
#20255 = ORIENTED_EDGE ( 'NONE', *, *, #6446, .F. ) ;
#20256 = DIRECTION ( 'NONE',  ( 0.000000000000000000, 0.000000000000000000, -1.000000000000000000 ) ) ;
#20257 = EDGE_LOOP ( 'NONE', ( #2146, #2706, #5445, #2426 ) ) ;
#20258 = CARTESIAN_POINT ( 'NONE',  ( -10.19618095414378622, -15.25966316918061416, 5.793793750180313396 ) ) ;
#20259 = CARTESIAN_POINT ( 'NONE',  ( 13.80207632871711532, -16.50074880709951586, 72.95245019206022619 ) ) ;
#20260 = VERTEX_POINT ( 'NONE', #12809 ) ;
#20261 = CARTESIAN_POINT ( 'NONE',  ( -10.00000000000000000, 0.000000000000000000, 0.000000000000000000 ) ) ;
#20262 = ORIENTED_EDGE ( 'NONE', *, *, #6924, .F. ) ;
#20263 = LINE ( 'NONE', #8722, #13574 ) ;
#20264 = CARTESIAN_POINT ( 'NONE',  ( 0.000000000000000000, 0.000000000000000000, 84.99999999999998579 ) ) ;
#20265 = CARTESIAN_POINT ( 'NONE',  ( 50.00000000000000000, -159.9999999999999716, 53.99496054166690584 ) ) ;
#20266 = EDGE_LOOP ( 'NONE', ( #19800, #6962, #4890, #9906 ) ) ;
#20267 = DIRECTION ( 'NONE',  ( 0.000000000000000000, 0.4999999999999992784, -0.8660254037844389297 ) ) ;
#20268 = DIRECTION ( 'NONE',  ( -0.000000000000000000, -0.000000000000000000, -1.000000000000000000 ) ) ;
#20269 = CARTESIAN_POINT ( 'NONE',  ( 10.19618095414378622, 15.25966316918061239, -8.343706249819691223 ) ) ;
#20270 = DIRECTION ( 'NONE',  ( -1.000000000000000000, -0.000000000000000000, -0.000000000000000000 ) ) ;
#20271 = DIRECTION ( 'NONE',  ( -1.000000000000000000, 0.000000000000000000, 0.000000000000000000 ) ) ;
#20272 = CARTESIAN_POINT ( 'NONE',  ( -1.343452921478824119E-09, -11.17563879731705789, -9.426140249352577882 ) ) ;
#20273 = ORIENTED_EDGE ( 'NONE', *, *, #9365, .T. ) ;
#20274 = ADVANCED_FACE ( 'NONE', ( #14803, #19353, #11199, #1569, #4838, #19564 ), #16384, .F. ) ;
#20275 = CARTESIAN_POINT ( 'NONE',  ( -10.00000000000000000, 0.000000000000000000, 0.000000000000000000 ) ) ;
#20276 = ORIENTED_EDGE ( 'NONE', *, *, #1702, .T. ) ;
#20277 = CARTESIAN_POINT ( 'NONE',  ( -3.872723063507617525, -21.16211945945224571, -70.72147569179591642 ) ) ;
#20278 = EDGE_LOOP ( 'NONE', ( #16087, #18445 ) ) ;
#20279 = CARTESIAN_POINT ( 'NONE',  ( -6.888301780572501976, 16.62983158603122291, -7.911762499819688266 ) ) ;
#20280 = LINE ( 'NONE', #18386, #208 ) ;
#20281 = PLANE ( 'NONE',  #2938 ) ;
#20282 = VERTEX_POINT ( 'NONE', #3445 ) ;
#20283 = CARTESIAN_POINT ( 'NONE',  ( -12.50000000000000533, 0.000000000000000000, 126.0000000000000000 ) ) ;
#20284 = EDGE_LOOP ( 'NONE', ( #7092, #9472, #15448 ) ) ;
#20285 = DIRECTION ( 'NONE',  ( 0.000000000000000000, 0.000000000000000000, -1.000000000000000000 ) ) ;
#20286 = VERTEX_POINT ( 'NONE', #4735 ) ;
#20287 = CIRCLE ( 'NONE', #14563, 27.60000000002759890 ) ;
#20288 = CARTESIAN_POINT ( 'NONE',  ( 0.000000000000000000, 0.000000000000000000, -5.600000000000000533 ) ) ;
#20289 = CARTESIAN_POINT ( 'NONE',  ( 20.00000000000000355, 0.000000000000000000, 7.500000000000000000 ) ) ;
#20290 = CONTEXT_DEPENDENT_SHAPE_REPRESENTATION ( #3044, #14905 ) ;
#20291 = CARTESIAN_POINT ( 'NONE',  ( -2.943691928843437999, -14.79893867722910450, -0.4589268311584565052 ) ) ;
#20292 = ORIENTED_EDGE ( 'NONE', *, *, #978, .F. ) ;
#20293 = EDGE_CURVE ( 'NONE', #3130, #4449, #11102, .T. ) ;
#20294 = CARTESIAN_POINT ( 'NONE',  ( -4.000000000000000000, 0.000000000000000000, -5.599999999999999645 ) ) ;
#20295 = ORIENTED_EDGE ( 'NONE', *, *, #9237, .T. ) ;
#20296 = DIRECTION ( 'NONE',  ( 0.000000000000000000, 0.000000000000000000, 1.000000000000000000 ) ) ;
#20297 = CARTESIAN_POINT ( 'NONE',  ( 6.888301784570727726, 16.62983158437509701, 10.21176250018031162 ) ) ;
#20298 = DIRECTION ( 'NONE',  ( -1.000000000000000000, 0.000000000000000000, 0.000000000000000000 ) ) ;
#20299 = CARTESIAN_POINT ( 'NONE',  ( 0.000000000000000000, -60.40676135667455071, 23.56039007469017221 ) ) ;
#20300 = EDGE_CURVE ( 'NONE', #14747, #16465, #19156, .T. ) ;
#20301 = ADVANCED_FACE ( 'NONE', ( #17884 ), #16186, .T. ) ;
#20302 = ORIENTED_EDGE ( 'NONE', *, *, #13067, .T. ) ;
#20303 = PLANE ( 'NONE',  #15808 ) ;
#20304 = CARTESIAN_POINT ( 'NONE',  ( -17.50000000000000355, 2.143131898507868643E-15, 166.0000000000000000 ) ) ;
#20305 = AXIS2_PLACEMENT_3D ( 'NONE', #13388, #18149, #3818 ) ;
#20306 = ORIENTED_EDGE ( 'NONE', *, *, #4818, .F. ) ;
#20307 = CARTESIAN_POINT ( 'NONE',  ( 18.08416879489398355, -14.22778436779400124, -80.18931099398717777 ) ) ;
#20308 = EDGE_LOOP ( 'NONE', ( #13956, #17459, #6448, #307, #12204, #20312 ) ) ;
#20309 = DIRECTION ( 'NONE',  ( 0.000000000000000000, -0.8878852184023702243, -0.4600650377311618633 ) ) ;
#20310 = CARTESIAN_POINT ( 'NONE',  ( 15.25966316918061239, -10.19618095414378445, -15.41245624981969087 ) ) ;
#20311 = ORIENTED_EDGE ( 'NONE', *, *, #9754, .F. ) ;
#20312 = ORIENTED_EDGE ( 'NONE', *, *, #7957, .F. ) ;
#20313 = CARTESIAN_POINT ( 'NONE',  ( 19.99999999999999645, 39.37110852956814000, 51.51683813304883586 ) ) ;
#20314 = CARTESIAN_POINT ( 'NONE',  ( 0.000000000000000000, 0.000000000000000000, 0.000000000000000000 ) ) ;
#20315 = CIRCLE ( 'NONE', #13902, 72.00000000007199219 ) ;
#20316 = PLANE ( 'NONE',  #19024 ) ;
#20317 = DIRECTION ( 'NONE',  ( 0.000000000000000000, 0.000000000000000000, -1.000000000000000000 ) ) ;
#20318 = DIRECTION ( 'NONE',  ( 1.000000000000000000, 0.000000000000000000, 0.000000000000000000 ) ) ;
#20319 = CARTESIAN_POINT ( 'NONE',  ( -3.580422610670018990, 18.00000000043041481, 11.23276875018031085 ) ) ;
#20320 = CARTESIAN_POINT ( 'NONE',  ( 4.248408730893249441, 6.358192987158595599, -13.68395624981969050 ) ) ;
#20321 = VECTOR ( 'NONE', #19, 1000.000000000000000 ) ;
#20322 = ORIENTED_EDGE ( 'NONE', *, *, #7645, .T. ) ;
#20323 = DIRECTION ( 'NONE',  ( 0.000000000000000000, 0.000000000000000000, 1.000000000000000000 ) ) ;
#20324 = CARTESIAN_POINT ( 'NONE',  ( 14.79893867793683349, 2.943691925285396582, 19.25267683151907505 ) ) ;
#20325 = CARTESIAN_POINT ( 'NONE',  ( 9.999999999999998224, -27.80658314415180499, -66.41380830714152239 ) ) ;
#20326 = ADVANCED_FACE ( 'NONE', ( #1868, #3042, #17977, #279, #9614 ), #15965, .T. ) ;
#20327 = ORIENTED_EDGE ( 'NONE', *, *, #20199, .T. ) ;
#20328 = LINE ( 'NONE', #15475, #3776 ) ;
#20329 = ADVANCED_FACE ( 'NONE', ( #883, #2683 ), #19656, .F. ) ;
#20330 = CARTESIAN_POINT ( 'NONE',  ( -16.62983158437510056, 6.888301784570729502, -18.51488749981968951 ) ) ;
#20331 = CARTESIAN_POINT ( 'NONE',  ( 0.000000000000000000, 56.42118728228200553, -32.77318456705383198 ) ) ;
#20332 = ORIENTED_EDGE ( 'NONE', *, *, #16263, .F. ) ;
#20333 = CARTESIAN_POINT ( 'NONE',  ( 0.000000000000000000, 0.000000000000000000, -5.599999999999999645 ) ) ;
#20334 = ORIENTED_EDGE ( 'NONE', *, *, #5970, .T. ) ;
#20335 = CARTESIAN_POINT ( 'NONE',  ( 36.39485347990547837, -22.16933930360253768, -75.72923816920850015 ) ) ;
#20336 = DIRECTION ( 'NONE',  ( 1.000000000000000000, -0.000000000000000000, 0.000000000000000000 ) ) ;
#20337 = VERTEX_POINT ( 'NONE', #8929 ) ;
#20338 = CIRCLE ( 'NONE', #18657, 2.649999999999992806 ) ;
#20339 = EDGE_CURVE ( 'NONE', #17908, #15704, #7694, .T. ) ;
#20340 = EDGE_LOOP ( 'NONE', ( #12154, #14910 ) ) ;
#20341 = DIRECTION ( 'NONE',  ( -0.4999999999999918954, 0.8660254037844433705, 0.000000000000000000 ) ) ;
#20342 =( LENGTH_UNIT ( ) NAMED_UNIT ( * ) SI_UNIT ( .MILLI., .METRE. ) );
#20343 = STYLED_ITEM ( 'NONE', ( #12525 ), #17220 ) ;
#20344 = DIRECTION ( 'NONE',  ( -1.000000000000000000, 0.000000000000000000, -0.000000000000000000 ) ) ;
#20345 = CYLINDRICAL_SURFACE ( 'NONE', #11225, 27.60000000002759890 ) ;
#20346 = SHAPE_REPRESENTATION ( 'needle roller bearing_nh_iso_ISO 3245 - 1532D - 14,SI,NC,14', ( #12461 ), #2252 ) ;
#20347 = VECTOR ( 'NONE', #17607, 1000.000000000000000 ) ;
#20348 = EDGE_CURVE ( 'NONE', #19645, #8741, #19860, .T. ) ;
#20349 = AXIS2_PLACEMENT_3D ( 'NONE', #8757, #706, #19982 ) ;
#20350 = CARTESIAN_POINT ( 'NONE',  ( 6.929096494179676213, 2.870125741905210415, -9.640262499819689523 ) ) ;
#20351 = LINE ( 'NONE', #7424, #9868 ) ;
#20352 = VECTOR ( 'NONE', #2528, 1000.000000000000000 ) ;
#20353 = DIRECTION ( 'NONE',  ( 0.000000000000000000, -0.9422609221188167350, -0.3348796121709969875 ) ) ;
#20354 = LINE ( 'NONE', #18784, #9173 ) ;
#20355 = CARTESIAN_POINT ( 'NONE',  ( 6.250000000000054179, 10.82531754730546147, 46.00000000000000711 ) ) ;
#20356 = ADVANCED_FACE ( 'NONE', ( #5250 ), #373, .T. ) ;
#20357 = ORIENTED_EDGE ( 'NONE', *, *, #17151, .T. ) ;
#20358 = DIRECTION ( 'NONE',  ( 0.000000000000000000, 0.000000000000000000, 1.000000000000000000 ) ) ;
#20359 = ADVANCED_FACE ( 'NONE', ( #10745 ), #7439, .T. ) ;
#20360 = ORIENTED_EDGE ( 'NONE', *, *, #15915, .F. ) ;
#20361 = CARTESIAN_POINT ( 'NONE',  ( -6.888301780572501976, 16.62983158603122291, 9.033637500180313751 ) ) ;
#20362 = CARTESIAN_POINT ( 'NONE',  ( 21.39608139526260899, -2.344611746178262734, 83.84634603192272095 ) ) ;
#20363 = COLOUR_RGB ( '', 0.31764706, 0.68627451, 0.89019608) ;
#20364 = VERTEX_POINT ( 'NONE', #13820 ) ;
#20365 = DIRECTION ( 'NONE',  ( 0.000000000000000000, 0.000000000000000000, 1.000000000000000000 ) ) ;
#20366 = ORIENTED_EDGE ( 'NONE', *, *, #954, .T. ) ;
#20367 = EDGE_CURVE ( 'NONE', #14604, #3608, #11408, .T. ) ;
#20368 = CARTESIAN_POINT ( 'NONE',  ( 42.30813292954685068, -123.8249046810892082, 81.51046245632689136 ) ) ;
#20369 = DIRECTION ( 'NONE',  ( 0.000000000000000000, 0.000000000000000000, 1.000000000000000000 ) ) ;
#20370 = CYLINDRICAL_SURFACE ( 'NONE', #9411, 2.649999999999993694 ) ;
#20371 = VERTEX_POINT ( 'NONE', #6938 ) ;
#20372 = CARTESIAN_POINT ( 'NONE',  ( 7.500000000000000000, -9.015933403756339613E-10, -21.63629999981969121 ) ) ;
#20373 = AXIS2_PLACEMENT_3D ( 'NONE', #10772, #13523, #15525 ) ;
#20374 = CIRCLE ( 'NONE', #1439, 72.00000000007199219 ) ;
#20375 = CIRCLE ( 'NONE', #16321, 10.00000000000000178 ) ;
#20376 = LINE ( 'NONE', #14038, #217 ) ;
#20377 = CARTESIAN_POINT ( 'NONE',  ( -12.72792205982779556, 12.72792206288790773, -19.83042499981969087 ) ) ;
#20378 = LINE ( 'NONE', #10648, #3850 ) ;
#20379 = CARTESIAN_POINT ( 'NONE',  ( 6.249999999999902300, -10.82531754730554496, 43.00000000000000000 ) ) ;
#20380 = ORIENTED_EDGE ( 'NONE', *, *, #8821, .F. ) ;
#20381 = ADVANCED_FACE ( 'NONE', ( #12217 ), #3657, .T. ) ;
#20382 = ADVANCED_FACE ( 'NONE', ( #17097, #13423, #10524, #5351 ), #10639, .F. ) ;
#20383 = LINE ( 'NONE', #18488, #5942 ) ;
#20384 = FACE_OUTER_BOUND ( 'NONE', #13167, .T. ) ;
#20385 = ORIENTED_EDGE ( 'NONE', *, *, #17299, .T. ) ;
#20386 = VECTOR ( 'NONE', #11320, 1000.000000000000000 ) ;
#20387 = CARTESIAN_POINT ( 'NONE',  ( -19.00859264729083620, -10.06624177801187869, -77.01193977728050299 ) ) ;
#20388 = CARTESIAN_POINT ( 'NONE',  ( 19.99999999999999645, 3.141410481201071914, 65.17333458706188765 ) ) ;
#20389 = CIRCLE ( 'NONE', #11259, 10.85999999999999410 ) ;
#20390 = ORIENTED_EDGE ( 'NONE', *, *, #12189, .T. ) ;
#20391 = AXIS2_PLACEMENT_3D ( 'NONE', #8136, #17692, #16201 ) ;
#20392 = CARTESIAN_POINT ( 'NONE',  ( -6.888301784570738384, -16.62983158437509346, -11.44613749981969164 ) ) ;
#20393 = ADVANCED_FACE ( 'NONE', ( #16980 ), #18684, .T. ) ;
#20394 = AXIS2_PLACEMENT_3D ( 'NONE', #14525, #3176, #6352 ) ;
#20395 = DIRECTION ( 'NONE',  ( -1.000000000000000000, 0.000000000000000000, 0.000000000000000000 ) ) ;
#20396 = FACE_BOUND ( 'NONE', #11478, .T. ) ;
#20397 = ORIENTED_EDGE ( 'NONE', *, *, #1665, .T. ) ;
#20398 = DIRECTION ( 'NONE',  ( 0.000000000000000000, 0.6310879443260538624, -0.7757112907044189098 ) ) ;
#20399 = ORIENTED_EDGE ( 'NONE', *, *, #16960, .F. ) ;
#20400 = LINE ( 'NONE', #18823, #6494 ) ;
#20401 = ORIENTED_EDGE ( 'NONE', *, *, #17918, .T. ) ;
#20402 = EDGE_CURVE ( 'NONE', #16141, #13626, #6004, .T. ) ;
#20403 = CARTESIAN_POINT ( 'NONE',  ( 6.165579999999999394, 0.000000000000000000, 0.000000000000000000 ) ) ;
#20404 = VECTOR ( 'NONE', #9595, 1000.000000000000000 ) ;
#20405 = CIRCLE ( 'NONE', #8545, 27.60000000002760601 ) ;
#20406 = CARTESIAN_POINT ( 'NONE',  ( 30.00000000000000000, -50.00000000000000000, 71.93747284969079203 ) ) ;
#20407 = CIRCLE ( 'NONE', #12288, 2.649999999999994582 ) ;
#20408 = CARTESIAN_POINT ( 'NONE',  ( 8.382925371439633011, 12.54593441562640876, -4.582364331158456316 ) ) ;
#20409 = EDGE_LOOP ( 'NONE', ( #17914, #17756, #17778, #7247 ) ) ;
#20410 = CYLINDRICAL_SURFACE ( 'NONE', #19761, 72.00000000007199219 ) ;
#20411 = ORIENTED_EDGE ( 'NONE', *, *, #12581, .F. ) ;
#20412 = AXIS2_PLACEMENT_3D ( 'NONE', #4448, #12515, #12300 ) ;
#20413 = CARTESIAN_POINT ( 'NONE',  ( -14.65527575808362037, -15.74483652605746009, 79.18672471502033261 ) ) ;
#20414 = VECTOR ( 'NONE', #2239, 1000.000000000000000 ) ;
#20415 = CARTESIAN_POINT ( 'NONE',  ( -10.19618095047497874, 15.25966317163202746, 8.739106250180311619 ) ) ;
#20416 = DIRECTION ( 'NONE',  ( 0.000000000000000000, 0.8169698930104393186, 0.5766803221148710801 ) ) ;
#20417 = DIRECTION ( 'NONE',  ( -1.000000000000000000, 0.000000000000000000, 0.000000000000000000 ) ) ;
#20418 = AXIS2_PLACEMENT_3D ( 'NONE', #17563, #6202, #12797 ) ;
#20419 = CIRCLE ( 'NONE', #17378, 27.60000000002759535 ) ;
#20420 = EDGE_LOOP ( 'NONE', ( #10446, #11640, #11615, #1924 ) ) ;
#20421 = DIRECTION ( 'NONE',  ( 1.000000000000000000, 0.000000000000000000, 0.000000000000000000 ) ) ;
#20422 = FACE_OUTER_BOUND ( 'NONE', #4064, .T. ) ;
#20423 = B_SPLINE_CURVE_WITH_KNOTS ( 'NONE', 3,
 ( #5319, #11787, #3716, #2368, #10322, #8729 ),
 .UNSPECIFIED., .F., .F.,
 ( 4, 2, 4 ),
 ( 0.004120275011746842714, 0.005288420935197119671, 0.006456566858647395761 ),
 .UNSPECIFIED. ) ;
#20424 = ORIENTED_EDGE ( 'NONE', *, *, #6716, .F. ) ;
#20425 = CARTESIAN_POINT ( 'NONE',  ( 22.32918011041974893, -5.620274625700770521, -87.66817617122062245 ) ) ;
#20426 = EDGE_CURVE ( 'NONE', #2965, #20728, #5664, .T. ) ;
#20427 = CARTESIAN_POINT ( 'NONE',  ( -30.00000000000000000, 36.35083268962915781, 50.00000000000000000 ) ) ;
#20428 = CARTESIAN_POINT ( 'NONE',  ( 12.72792205982779379, -12.72792206288790950, -5.692924999819690690 ) ) ;
#20429 = EDGE_CURVE ( 'NONE', #3338, #5717, #16493, .T. ) ;
#20430 = ORIENTED_EDGE ( 'NONE', *, *, #2739, .F. ) ;
#20431 = CIRCLE ( 'NONE', #2836, 2.649999999999988365 ) ;
#20432 = ORIENTED_EDGE ( 'NONE', *, *, #17750, .T. ) ;
#20433 = DIRECTION ( 'NONE',  ( 0.000000000000000000, 0.000000000000000000, -1.000000000000000000 ) ) ;
#20434 = AXIS2_PLACEMENT_3D ( 'NONE', #1430, #7880, #6076 ) ;
#20435 = CARTESIAN_POINT ( 'NONE',  ( 0.000000000000000000, -44.69367065308685483, 56.44887778834731762 ) ) ;
#20436 = CARTESIAN_POINT ( 'NONE',  ( 19.99999999999999645, 0.000000000000000000, 0.000000000000000000 ) ) ;
#20437 = CYLINDRICAL_SURFACE ( 'NONE', #3128, 27.60000000002759890 ) ;
#20438 = CARTESIAN_POINT ( 'NONE',  ( 18.00000000000000355, -2.163824016901520597E-09, 4.458550000180308892 ) ) ;
#20439 = CIRCLE ( 'NONE', #17396, 7.567219999999999835 ) ;
#20440 = VECTOR ( 'NONE', #19409, 1000.000000000000000 ) ;
#20441 = CIRCLE ( 'NONE', #19104, 3.199999999999994404 ) ;
#20442 = UNCERTAINTY_MEASURE_WITH_UNIT (LENGTH_MEASURE( 1.000000000000000082E-05 ), #18267, 'distance_accuracy_value', 'NONE');
#20443 = CARTESIAN_POINT ( 'NONE',  ( -7.500000000000007994, 9.015942588607339023E-10, -16.92379999981968908 ) ) ;
#20444 = ORIENTED_EDGE ( 'NONE', *, *, #12068, .F. ) ;
#20445 = CARTESIAN_POINT ( 'NONE',  ( -1.491842756249033286, -7.499999999820668783, 18.71448125018031661 ) ) ;
#20446 = CARTESIAN_POINT ( 'NONE',  ( -2.222972771497743416, -11.17563879704981566, -25.67932850028680747 ) ) ;
#20447 = AXIS2_PLACEMENT_3D ( 'NONE', #4274, #15608, #1111 ) ;
#20448 = FACE_BOUND ( 'NONE', #389, .T. ) ;
#20449 = ORIENTED_EDGE ( 'NONE', *, *, #8624, .T. ) ;
#20450 = DIRECTION ( 'NONE',  ( -1.000000000000000000, 0.000000000000000000, 0.000000000000000000 ) ) ;
#20451 = CARTESIAN_POINT ( 'NONE',  ( 18.00000000043041126, 3.580422610670019434, -14.68598124981969022 ) ) ;
#20452 = CARTESIAN_POINT ( 'NONE',  ( 0.000000000000000000, 0.000000000000000000, -0.2800830152838832965 ) ) ;
#20453 = ORIENTED_EDGE ( 'NONE', *, *, #12703, .T. ) ;
#20454 = CARTESIAN_POINT ( 'NONE',  ( 0.000000000000000000, 0.000000000000000000, -5.599999999999999645 ) ) ;
#20455 = VERTEX_POINT ( 'NONE', #19769 ) ;
#20456 = AXIS2_PLACEMENT_3D ( 'NONE', #18358, #2256, #462 ) ;
#20457 = CARTESIAN_POINT ( 'NONE',  ( 0.000000000000000000, -64.36139404985944168, -32.27399814043941007 ) ) ;
#20458 = CARTESIAN_POINT ( 'NONE',  ( 0.000000000000000000, -31.98952867950285395, -56.39803944231618971 ) ) ;
#20459 = VERTEX_POINT ( 'NONE', #11720 ) ;
#20460 = ORIENTED_EDGE ( 'NONE', *, *, #19434, .T. ) ;
#20461 = CARTESIAN_POINT ( 'NONE',  ( 9.000000000000007105, -85.00000000000000000, 5.000000000000000000 ) ) ;
#20462 = CARTESIAN_POINT ( 'NONE',  ( 19.99999999999999645, -38.69327817041739337, -52.53819777490673459 ) ) ;
#20463 = ADVANCED_FACE ( 'NONE', ( #18190, #2069 ), #8523, .F. ) ;
#20464 = CARTESIAN_POINT ( 'NONE',  ( 14.50000000000000888, -85.00000000000000000, 19.00000000000000000 ) ) ;
#20465 = AXIS2_PLACEMENT_3D ( 'NONE', #6974, #5385, #13463 ) ;
#20466 = CARTESIAN_POINT ( 'NONE',  ( -7.500000000179339210, -1.491842754445842800, -23.48323124981969201 ) ) ;
#20467 = CARTESIAN_POINT ( 'NONE',  ( 19.99999999999999645, 51.43306257653197378, -40.15061736769512635 ) ) ;
#20468 = CARTESIAN_POINT ( 'NONE',  ( 9.470358143689576735, -1.138454911109686870E-09, -11.01577170245055370 ) ) ;
#20469 = DIRECTION ( 'NONE',  ( 0.000000000000000000, 1.040834085586084454E-15, -1.000000000000000000 ) ) ;
#20470 = ADVANCED_FACE ( 'NONE', ( #14348 ), #17309, .F. ) ;
#20471 = ORIENTED_EDGE ( 'NONE', *, *, #20226, .T. ) ;
#20472 = LINE ( 'NONE', #16129, #12250 ) ;
#20473 = EDGE_LOOP ( 'NONE', ( #11668, #15089, #13911, #12138 ) ) ;
#20474 = CARTESIAN_POINT ( 'NONE',  ( -16.62983158603122291, -6.888301780572501087, -12.17261249981968874 ) ) ;
#20475 = DIRECTION ( 'NONE',  ( 0.000000000000000000, 0.000000000000000000, 1.000000000000000000 ) ) ;
#20476 = DIRECTION ( 'NONE',  ( -0.000000000000000000, -0.000000000000000000, -1.000000000000000000 ) ) ;
#20477 = EDGE_LOOP ( 'NONE', ( #1314, #248, #6382, #13020, #7339 ) ) ;
#20478 = DIRECTION ( 'NONE',  ( -0.000000000000000000, -0.000000000000000000, 1.000000000000000000 ) ) ;
#20479 = ORIENTED_EDGE ( 'NONE', *, *, #4725, .T. ) ;
#20480 = DIRECTION ( 'NONE',  ( 0.000000000000000000, 0.000000000000000000, 1.000000000000000000 ) ) ;
#20481 = CARTESIAN_POINT ( 'NONE',  ( 9.999999999999998224, -8.857208570069305509, -71.45313048675095047 ) ) ;
#20482 = CARTESIAN_POINT ( 'NONE',  ( 2.500000000000000000, -2.629050547790028551E-15, -2.041999999999999815 ) ) ;
#20483 = ORIENTED_EDGE ( 'NONE', *, *, #6089, .T. ) ;
#20484 = CARTESIAN_POINT ( 'NONE',  ( 0.000000000000000000, 64.36139404986010959, -32.27399814043809556 ) ) ;
#20485 = CIRCLE ( 'NONE', #18814, 27.60000000002759890 ) ;
#20486 = CARTESIAN_POINT ( 'NONE',  ( 0.000000000000000000, -38.22257254261782577, 61.01667762370126269 ) ) ;
#20487 = DIRECTION ( 'NONE',  ( -1.000000000000000000, 0.000000000000000000, 0.000000000000000000 ) ) ;
#20488 = CARTESIAN_POINT ( 'NONE',  ( 21.00000000000000355, 0.000000000000000000, 0.000000000000000000 ) ) ;
#20489 = ADVANCED_FACE ( 'NONE', ( #7657 ), #14033, .T. ) ;
#20490 = EDGE_CURVE ( 'NONE', #6927, #19685, #19115, .T. ) ;
#20491 = DIRECTION ( 'NONE',  ( 0.000000000000000000, -1.224646799147353454E-16, 1.000000000000000000 ) ) ;
#20492 = VERTEX_POINT ( 'NONE', #20793 ) ;
#20493 = CARTESIAN_POINT ( 'NONE',  ( -1.660531772554312280, 3.660093687634848436, 2.744386749103932310E-15 ) ) ;
#20494 = VECTOR ( 'NONE', #14507, 1000.000000000000000 ) ;
#20495 = ADVANCED_FACE ( 'NONE', ( #9357 ), #1318, .F. ) ;
#20496 = CARTESIAN_POINT ( 'NONE',  ( 9.999999999999998224, -67.51707036274430607, 25.00890260772354878 ) ) ;
#20497 = ORIENTED_EDGE ( 'NONE', *, *, #17866, .F. ) ;
#20498 = DIRECTION ( 'NONE',  ( 1.000000000000000000, 0.000000000000000000, 0.000000000000000000 ) ) ;
#20499 = CARTESIAN_POINT ( 'NONE',  ( 2.500000000000000000, -1.178949249685218303, -2.041999999999998039 ) ) ;
#20500 = MECHANICAL_DESIGN_GEOMETRIC_PRESENTATION_REPRESENTATION (  '', ( #16758 ), #11370 ) ;
#20501 = VERTEX_POINT ( 'NONE', #15819 ) ;
#20502 = CARTESIAN_POINT ( 'NONE',  ( 10.19618095047497874, -15.25966317163203279, -12.91879374981968631 ) ) ;
#20503 = CARTESIAN_POINT ( 'NONE',  ( 19.99999999999999645, -11.98658579560543025, -64.13855129306480762 ) ) ;
#20504 = DIRECTION ( 'NONE',  ( 0.000000000000000000, 0.000000000000000000, 1.000000000000000000 ) ) ;
#20505 = ORIENTED_EDGE ( 'NONE', *, *, #16627, .F. ) ;
#20506 = DIRECTION ( 'NONE',  ( -1.000000000000000000, 0.000000000000000000, 0.000000000000000000 ) ) ;
#20507 = VERTEX_POINT ( 'NONE', #7764 ) ;
#20508 = CARTESIAN_POINT ( 'NONE',  ( 4.000000000000003553, 2.309401076758524685, -0.3572655899081733644 ) ) ;
#20509 = EDGE_CURVE ( 'NONE', #6520, #17663, #12444, .T. ) ;
#20510 = EDGE_LOOP ( 'NONE', ( #18492, #18674, #7744, #19719 ) ) ;
#20511 = EDGE_CURVE ( 'NONE', #5396, #9946, #20908, .T. ) ;
#20512 = CARTESIAN_POINT ( 'NONE',  ( 33.22510083995761221, -115.8989469114827955, 76.12820955576133031 ) ) ;
#20513 = VECTOR ( 'NONE', #3651, 1000.000000000000000 ) ;
#20514 = CIRCLE ( 'NONE', #7639, 27.60000000002759890 ) ;
#20515 = EDGE_CURVE ( 'NONE', #19384, #7136, #7978, .T. ) ;
#20516 = CARTESIAN_POINT ( 'NONE',  ( 19.99999999999999645, -14.55863677812078016, -63.60407295269120453 ) ) ;
#20517 = CARTESIAN_POINT ( 'NONE',  ( 12.54593441764187567, 8.382925368423276069, 5.431698168841543328 ) ) ;
#20518 = VERTEX_POINT ( 'NONE', #10839 ) ;
#20519 = VECTOR ( 'NONE', #5425, 1000.000000000000000 ) ;
#20520 = CARTESIAN_POINT ( 'NONE',  ( 0.000000000000000000, -51.81019761368347787, 38.98425606966041101 ) ) ;
#20521 = ORIENTED_EDGE ( 'NONE', *, *, #10894, .F. ) ;
#20522 = CARTESIAN_POINT ( 'NONE',  ( 0.000000000000000000, -10.74906464462068456, -71.19310085447979475 ) ) ;
#20523 = CARTESIAN_POINT ( 'NONE',  ( -15.25966316918061416, 10.19618095414378445, 8.150043750180310909 ) ) ;
#20524 = VECTOR ( 'NONE', #10722, 1000.000000000000000 ) ;
#20525 = CARTESIAN_POINT ( 'NONE',  ( 1.491842756249029289, 7.499999999820664343, -20.53791874981969912 ) ) ;
#20526 = CARTESIAN_POINT ( 'NONE',  ( 43.62500077266425791, -125.0000000000000000, 90.00000000000002842 ) ) ;
#20527 = CIRCLE ( 'NONE', #7671, 11.50000000000000000 ) ;
#20528 = AXIS2_PLACEMENT_3D ( 'NONE', #13854, #5783, #19705 ) ;
#20529 = ORIENTED_EDGE ( 'NONE', *, *, #1609, .F. ) ;
#20530 = DIRECTION ( 'NONE',  ( 0.000000000000000000, 0.000000000000000000, 1.000000000000000000 ) ) ;
#20531 = DIRECTION ( 'NONE',  ( -0.000000000000000000, -0.000000000000000000, 1.000000000000000000 ) ) ;
#20532 = VERTEX_POINT ( 'NONE', #2784 ) ;
#20533 = FACE_OUTER_BOUND ( 'NONE', #18065, .T. ) ;
#20534 = CARTESIAN_POINT ( 'NONE',  ( 4.248408729364576253, -6.358192988180015881, 1.846456250180306791 ) ) ;
#20535 = CARTESIAN_POINT ( 'NONE',  ( 12.72792205982779379, -12.72792206288790950, -15.11792499981969051 ) ) ;
#20536 = VECTOR ( 'NONE', #19614, 1000.000000000000000 ) ;
#20537 = VERTEX_POINT ( 'NONE', #9252 ) ;
#20538 = DIRECTION ( 'NONE',  ( 1.000000000000000000, 0.000000000000000000, 0.000000000000000000 ) ) ;
#20539 = AXIS2_PLACEMENT_3D ( 'NONE', #20109, #628, #13769 ) ;
#20540 = DIRECTION ( 'NONE',  ( -1.000000000000000000, 0.000000000000000000, 0.000000000000000000 ) ) ;
#20541 = VECTOR ( 'NONE', #1897, 1000.000000000000000 ) ;
#20542 = DIRECTION ( 'NONE',  ( -0.000000000000000000, 0.000000000000000000, 1.000000000000000000 ) ) ;
#20543 = DIRECTION ( 'NONE',  ( -1.000000000000000000, 0.000000000000000000, 0.000000000000000000 ) ) ;
#20544 = DIRECTION ( 'NONE',  ( 1.000000000000000000, 0.000000000000000000, 0.000000000000000000 ) ) ;
#20545 = CARTESIAN_POINT ( 'NONE',  ( -18.00000000043041481, -3.580422610670022987, 8.876518750180311557 ) ) ;
#20546 = AXIS2_PLACEMENT_3D ( 'NONE', #10883, #4086, #20530 ) ;
#20547 = CARTESIAN_POINT ( 'NONE',  ( 6.358192988180019434, 4.248408729364581582, -13.09489374981968801 ) ) ;
#20548 = ORIENTED_EDGE ( 'NONE', *, *, #2912, .F. ) ;
#20549 = DIRECTION ( 'NONE',  ( 0.000000000000000000, -1.040834085586084454E-15, 1.000000000000000000 ) ) ;
#20550 = CARTESIAN_POINT ( 'NONE',  ( -12.54593441764187034, -8.382925368423267187, 4.526114331519074163 ) ) ;
#20551 = ADVANCED_FACE ( 'NONE', ( #11153 ), #6063, .T. ) ;
#20552 = CIRCLE ( 'NONE', #20882, 72.00000000007199219 ) ;
#20553 = FACE_OUTER_BOUND ( 'NONE', #6913, .T. ) ;
#20554 = VERTEX_POINT ( 'NONE', #19001 ) ;
#20555 = CARTESIAN_POINT ( 'NONE',  ( 0.000000000000000000, 0.000000000000000000, -40.00000000000000000 ) ) ;
#20556 = AXIS2_PLACEMENT_3D ( 'NONE', #20313, #10696, #5795 ) ;
#20557 = CARTESIAN_POINT ( 'NONE',  ( 3.580422610670020322, -18.00000000043041126, -21.75473124981968809 ) ) ;
#20558 = DIRECTION ( 'NONE',  ( 0.000000000000000000, 0.000000000000000000, -1.000000000000000000 ) ) ;
#20559 = ORIENTED_EDGE ( 'NONE', *, *, #20685, .F. ) ;
#20560 = DIRECTION ( 'NONE',  ( 0.000000000000000000, -0.5195839500354229035, -0.8544194045464950094 ) ) ;
#20561 = AXIS2_PLACEMENT_3D ( 'NONE', #2744, #1172, #17055 ) ;
#20562 = ORIENTED_EDGE ( 'NONE', *, *, #14173, .T. ) ;
#20563 = CARTESIAN_POINT ( 'NONE',  ( 39.31722773736984067, -16.79517646696619693, -78.51518414706339399 ) ) ;
#20564 = DIRECTION ( 'NONE',  ( -1.000000000000000000, 0.000000000000000000, 0.000000000000000000 ) ) ;
#20565 = AXIS2_PLACEMENT_3D ( 'NONE', #5135, #11607, #11815 ) ;
#20566 = ORIENTED_EDGE ( 'NONE', *, *, #5075, .T. ) ;
#20567 = VERTEX_POINT ( 'NONE', #3096 ) ;
#20568 = CARTESIAN_POINT ( 'NONE',  ( 30.97876637327306071, -111.1959070590765748, -74.06233646255252268 ) ) ;
#20569 = CIRCLE ( 'NONE', #11434, 72.00000000007199219 ) ;
#20570 = CARTESIAN_POINT ( 'NONE',  ( -7.500000000000000000, 0.000000000000000000, 40.00000000000000000 ) ) ;
#20571 = ADVANCED_FACE ( 'NONE', ( #4588 ), #9558, .F. ) ;
#20572 = AXIS2_PLACEMENT_3D ( 'NONE', #153, #6606, #9592 ) ;
#20573 = DIRECTION ( 'NONE',  ( -1.000000000000000000, 0.000000000000000000, 0.000000000000000000 ) ) ;
#20574 = CARTESIAN_POINT ( 'NONE',  ( -9.474249098604506258, -6.330490856366290053, 13.19879649971320035 ) ) ;
#20575 = ADVANCED_FACE ( 'NONE', ( #14455 ), #7548, .F. ) ;
#20576 = CARTESIAN_POINT ( 'NONE',  ( 6.177131623262577698, 1.329966423874024758E-15, -10.85999999999999410 ) ) ;
#20577 = DIRECTION ( 'NONE',  ( 1.000000000000000000, -0.000000000000000000, -0.000000000000000000 ) ) ;
#20578 = ORIENTED_EDGE ( 'NONE', *, *, #9161, .F. ) ;
#20579 = DIRECTION ( 'NONE',  ( 1.000000000000000000, -0.000000000000000000, -0.000000000000000000 ) ) ;
#20580 = ORIENTED_EDGE ( 'NONE', *, *, #20607, .F. ) ;
#20581 = CARTESIAN_POINT ( 'NONE',  ( 16.62983158437509346, -6.888301784570739272, -15.70698749981968767 ) ) ;
#20582 = CARTESIAN_POINT ( 'NONE',  ( 18.66082225198899636, -10.69875493221384311, 76.55584491636111011 ) ) ;
#20583 = EDGE_LOOP ( 'NONE', ( #3472, #18583, #2605, #10744, #16542 ) ) ;
#20584 = EDGE_CURVE ( 'NONE', #17275, #16282, #1415, .T. ) ;
#20585 = DIRECTION ( 'NONE',  ( -1.000000000000000000, -0.000000000000000000, -0.000000000000000000 ) ) ;
#20586 = EDGE_LOOP ( 'NONE', ( #4854, #4295, #10351, #9440 ) ) ;
#20587 = CARTESIAN_POINT ( 'NONE',  ( -9.850000000000012079, 3.245314017740477087E-16, 169.0000000000000000 ) ) ;
#20588 = CARTESIAN_POINT ( 'NONE',  ( 19.99999999999999645, 54.08351995568756365, -35.76369202524444546 ) ) ;
#20589 = CARTESIAN_POINT ( 'NONE',  ( 0.000000000000000000, 60.40676135667469282, -23.56039007468977431 ) ) ;
#20590 = ORIENTED_EDGE ( 'NONE', *, *, #1009, .T. ) ;
#20591 = LINE ( 'NONE', #17736, #6607 ) ;
#20592 = DIRECTION ( 'NONE',  ( -1.000000000000000000, 0.000000000000000000, 0.000000000000000000 ) ) ;
#20593 = CARTESIAN_POINT ( 'NONE',  ( -2.163827323447877821E-09, -17.99999999999999645, -23.36479999981969158 ) ) ;
#20594 = CARTESIAN_POINT ( 'NONE',  ( 50.00000000000000000, -170.8299878242309546, -15.48896927112552824 ) ) ;
#20595 = PLANE ( 'NONE',  #9282 ) ;
#20596 = EDGE_LOOP ( 'NONE', ( #6686, #15928 ) ) ;
#20597 = CARTESIAN_POINT ( 'NONE',  ( -0.3263565795980851170, 4.430380094434251959, -0.2484800633750073040 ) ) ;
#20598 = DIRECTION ( 'NONE',  ( -1.000000000000000000, -0.000000000000000000, -0.000000000000000000 ) ) ;
#20599 = ORIENTED_EDGE ( 'NONE', *, *, #7668, .F. ) ;
#20600 = CARTESIAN_POINT ( 'NONE',  ( 0.000000000000000000, -0.9548212943370493200, 71.99366858485716136 ) ) ;
#20601 = CARTESIAN_POINT ( 'NONE',  ( 2.500000000000000000, 2.357898499370433054, -1.951563910473907981E-15 ) ) ;
#20602 = VERTEX_POINT ( 'NONE', #20117 ) ;
#20603 = CARTESIAN_POINT ( 'NONE',  ( 3.580422614997668340, 17.99999999956958519, -16.45316874981969235 ) ) ;
#20604 = FACE_OUTER_BOUND ( 'NONE', #7081, .T. ) ;
#20605 = CYLINDRICAL_SURFACE ( 'NONE', #13681, 2.649999999999993694 ) ;
#20606 = ORIENTED_EDGE ( 'NONE', *, *, #8157, .F. ) ;
#20607 = EDGE_CURVE ( 'NONE', #6801, #14238, #7707, .T. ) ;
#20608 = CARTESIAN_POINT ( 'NONE',  ( -54.64999999999999858, -99.99999999999998579, 5.000000000000000000 ) ) ;
#20609 = VERTEX_POINT ( 'NONE', #5924 ) ;
#20610 = DIRECTION ( 'NONE',  ( 0.000000000000000000, 0.000000000000000000, 1.000000000000000000 ) ) ;
#20611 = ADVANCED_FACE ( 'NONE', ( #18760 ), #16941, .T. ) ;
#20612 = VERTEX_POINT ( 'NONE', #9001 ) ;
#20613 = EDGE_CURVE ( 'NONE', #9255, #1354, #9661, .T. ) ;
#20614 = DIRECTION ( 'NONE',  ( 0.000000000000000000, -1.000000000000000000, -0.000000000000000000 ) ) ;
#20615 = DIRECTION ( 'NONE',  ( -1.000000000000000000, 0.000000000000000000, 0.000000000000000000 ) ) ;
#20616 = CARTESIAN_POINT ( 'NONE',  ( -12.54593441764187745, -8.382925368423274293, 0.7191981688415456375 ) ) ;
#20617 = ORIENTED_EDGE ( 'NONE', *, *, #15957, .T. ) ;
#20618 = CARTESIAN_POINT ( 'NONE',  ( 18.00000000000000000, -2.163824016901520184E-09, -23.81644999981969235 ) ) ;
#20619 = CARTESIAN_POINT ( 'NONE',  ( -6.165580000000000283, 0.000000000000000000, 0.000000000000000000 ) ) ;
#20620 = EDGE_LOOP ( 'NONE', ( #11117, #10939, #3763, #16921 ) ) ;
#20621 = CARTESIAN_POINT ( 'NONE',  ( 17.89279294550298260, -11.93604557640007613, 81.86420770708537020 ) ) ;
#20622 = EDGE_CURVE ( 'NONE', #742, #15420, #595, .T. ) ;
#20623 = CARTESIAN_POINT ( 'NONE',  ( 2.163825119083639120E-09, 17.99999999999999645, 9.622700000180310909 ) ) ;
#20624 = LINE ( 'NONE', #2825, #2067 ) ;
#20625 = CARTESIAN_POINT ( 'NONE',  ( 85.00002539999999840, 0.000000000000000000, 7.500000000000000000 ) ) ;
#20626 = EDGE_CURVE ( 'NONE', #19670, #3863, #19222, .T. ) ;
#20627 = EDGE_LOOP ( 'NONE', ( #6010, #17393, #7459, #10153 ) ) ;
#20628 = EDGE_CURVE ( 'NONE', #8629, #8808, #6675, .T. ) ;
#20629 = CARTESIAN_POINT ( 'NONE',  ( 19.99999999999999645, 56.42118728228154367, 32.77318456705460648 ) ) ;
#20630 = CARTESIAN_POINT ( 'NONE',  ( 24.99999999999999289, -30.00000000000000711, 44.99999999999998579 ) ) ;
#20631 = EDGE_LOOP ( 'NONE', ( #4239, #12211, #8893 ) ) ;
#20632 = DIRECTION ( 'NONE',  ( 1.000000000000000000, 0.000000000000000000, 0.000000000000000000 ) ) ;
#20633 = DIRECTION ( 'NONE',  ( -1.648349939164583989E-16, 1.000000000000000000, 0.000000000000000000 ) ) ;
#20634 = EDGE_CURVE ( 'NONE', #1298, #540, #15469, .T. ) ;
#20635 = CARTESIAN_POINT ( 'NONE',  ( -15.25966316918061416, 10.19618095414378445, -20.12495624981969300 ) ) ;
#20636 = ORIENTED_EDGE ( 'NONE', *, *, #13641, .F. ) ;
#20637 = DIRECTION ( 'NONE',  ( -1.000000000000000000, 0.000000000000000000, 0.000000000000000000 ) ) ;
#20638 = CARTESIAN_POINT ( 'NONE',  ( 30.00000000000000000, -85.00000000000000000, -1.040949779275250179E-14 ) ) ;
#20639 = CARTESIAN_POINT ( 'NONE',  ( 0.000000000000000000, -63.05226888949902531, 15.11556105343437828 ) ) ;
#20640 = DIRECTION ( 'NONE',  ( -1.000000000000000000, 0.000000000000000000, 0.000000000000000000 ) ) ;
#20641 = DIRECTION ( 'NONE',  ( 0.000000000000000000, 0.000000000000000000, 1.000000000000000000 ) ) ;
#20642 = CARTESIAN_POINT ( 'NONE',  ( 10.19618095414378978, 15.25966316918061771, 12.41089375018030871 ) ) ;
#20643 = CARTESIAN_POINT ( 'NONE',  ( 2.000000000000027089, 3.464101615137739731, 0.000000000000000000 ) ) ;
#20644 = ORIENTED_EDGE ( 'NONE', *, *, #18534, .T. ) ;
#20645 = CYLINDRICAL_SURFACE ( 'NONE', #16167, 27.60000000002759890 ) ;
#20646 = ADVANCED_FACE ( 'NONE', ( #12174 ), #4110, .F. ) ;
#20647 = CARTESIAN_POINT ( 'NONE',  ( 1.779017513685135741E-09, 14.79893867758296544, 17.19095808151907789 ) ) ;
#20648 = AXIS2_PLACEMENT_3D ( 'NONE', #18570, #12721, #17591 ) ;
#20649 = ORIENTED_EDGE ( 'NONE', *, *, #14545, .F. ) ;
#20650 = LINE ( 'NONE', #11436, #1120 ) ;
#20651 = FACE_OUTER_BOUND ( 'NONE', #2808, .T. ) ;
#20652 = LINE ( 'NONE', #15678, #5998 ) ;
#20653 = ORIENTED_EDGE ( 'NONE', *, *, #5905, .T. ) ;
#20654 = CYLINDRICAL_SURFACE ( 'NONE', #14297, 2.649999999999993694 ) ;
#20655 = VERTEX_POINT ( 'NONE', #844 ) ;
#20656 = DIRECTION ( 'NONE',  ( -1.000000000000000000, 0.000000000000000000, -0.000000000000000000 ) ) ;
#20657 = CARTESIAN_POINT ( 'NONE',  ( 19.99999999999999645, 60.40676135667469282, -23.56039007468977431 ) ) ;
#20658 = AXIS2_PLACEMENT_3D ( 'NONE', #9375, #10759, #18596 ) ;
#20659 = ORIENTED_EDGE ( 'NONE', *, *, #14807, .T. ) ;
#20660 = EDGE_LOOP ( 'NONE', ( #2083, #3561, #13260, #4527, #18786 ) ) ;
#20661 = CARTESIAN_POINT ( 'NONE',  ( 39.99999999999997158, -122.3205080756887497, -80.28096411455980785 ) ) ;
#20662 = ADVANCED_FACE ( 'NONE', ( #11966 ), #4228, .T. ) ;
#20663 = CIRCLE ( 'NONE', #19643, 27.60000000002759890 ) ;
#20664 = DIRECTION ( 'NONE',  ( -1.000000000000000000, 0.000000000000000000, -0.000000000000000000 ) ) ;
#20665 = FACE_OUTER_BOUND ( 'NONE', #19154, .T. ) ;
#20666 = CARTESIAN_POINT ( 'NONE',  ( 6.330490856366294494, -9.474249098604513364, -10.30973399935257007 ) ) ;
#20667 = CARTESIAN_POINT ( 'NONE',  ( 6.358192988180013216, 4.248408729364577141, -19.35979374981969059 ) ) ;
#20668 = CARTESIAN_POINT ( 'NONE',  ( 10.00000000000000178, -160.0000000000000000, 70.00000000000000000 ) ) ;
#20669 = CARTESIAN_POINT ( 'NONE',  ( -12.50000000000000533, 0.000000000000000000, 46.00000000000000711 ) ) ;
#20670 = CARTESIAN_POINT ( 'NONE',  ( 19.99999999999999645, -71.76067541710854414, 5.865617076724380041 ) ) ;
#20671 = ORIENTED_EDGE ( 'NONE', *, *, #13374, .F. ) ;
#20672 = CYLINDRICAL_SURFACE ( 'NONE', #6820, 72.00000000007199219 ) ;
#20673 = ORIENTED_EDGE ( 'NONE', *, *, #15735, .F. ) ;
#20674 = CARTESIAN_POINT ( 'NONE',  ( 12.72792206288790950, 12.72792205982780089, -17.47417499981969158 ) ) ;
#20675 = CARTESIAN_POINT ( 'NONE',  ( 30.00000000000000000, 4.299168419249259188, -90.00000000000000000 ) ) ;
#20676 = AXIS2_PLACEMENT_3D ( 'NONE', #2863, #1070, #14319 ) ;
#20677 = ORIENTED_EDGE ( 'NONE', *, *, #5772, .T. ) ;
#20678 = DIRECTION ( 'NONE',  ( 0.000000000000000000, -0.3984010898462297390, -0.9172113015054581542 ) ) ;
#20679 = ORIENTED_EDGE ( 'NONE', *, *, #5367, .F. ) ;
#20680 = CARTESIAN_POINT ( 'NONE',  ( -21.35784117651625280, 26.35784117651607872, -120.0000000000000142 ) ) ;
#20681 = CARTESIAN_POINT ( 'NONE',  ( 19.99999999999999645, 0.000000000000000000, 0.000000000000000000 ) ) ;
#20682 = CARTESIAN_POINT ( 'NONE',  ( 6.999999999999999112, 7.118024431592597790E-15, 0.000000000000000000 ) ) ;
#20683 = ORIENTED_EDGE ( 'NONE', *, *, #17781, .T. ) ;
#20684 = DIRECTION ( 'NONE',  ( 0.000000000000000000, 0.000000000000000000, 1.000000000000000000 ) ) ;
#20685 = EDGE_CURVE ( 'NONE', #20728, #10182, #1292, .T. ) ;
#20686 = CYLINDRICAL_SURFACE ( 'NONE', #10371, 27.60000000002759535 ) ;
#20687 = DIRECTION ( 'NONE',  ( 0.000000000000000000, 0.000000000000000000, -1.000000000000000000 ) ) ;
#20688 = CARTESIAN_POINT ( 'NONE',  ( 52.50000000000000000, -30.00000000000000000, 5.000000000000000000 ) ) ;
#20689 = CIRCLE ( 'NONE', #4098, 65.24900000006525147 ) ;
#20690 = DIRECTION ( 'NONE',  ( -0.000000000000000000, -0.000000000000000000, 1.000000000000000000 ) ) ;
#20691 = AXIS2_PLACEMENT_3D ( 'NONE', #13451, #18311, #16518 ) ;
#20692 = EDGE_LOOP ( 'NONE', ( #974, #1531, #8426, #5541 ) ) ;
#20693 = LINE ( 'NONE', #3106, #19468 ) ;
#20694 = CARTESIAN_POINT ( 'NONE',  ( 0.000000000000000000, 2.357898499370433054, -1.951563910473907981E-15 ) ) ;
#20695 = EDGE_LOOP ( 'NONE', ( #4927, #8554, #19490, #3630, #17965 ) ) ;
#20696 = AXIS2_PLACEMENT_3D ( 'NONE', #1618, #6262, #9545 ) ;
#20697 = CARTESIAN_POINT ( 'NONE',  ( 50.00100000000000477, -85.00000000000000000, -9.000000000000005329 ) ) ;
#20698 = CARTESIAN_POINT ( 'NONE',  ( -11.50000000000000000, 0.000000000000000000, -68.00000000000000000 ) ) ;
#20699 = ORIENTED_EDGE ( 'NONE', *, *, #14351, .F. ) ;
#20700 = CARTESIAN_POINT ( 'NONE',  ( 15.25966317163202746, 10.19618095047498407, -15.27504374981969093 ) ) ;
#20701 = DIRECTION ( 'NONE',  ( -0.000000000000000000, -0.000000000000000000, -1.000000000000000000 ) ) ;
#20702 = CARTESIAN_POINT ( 'NONE',  ( 19.99999999999999645, -63.85430960833497949, 11.25592921604817676 ) ) ;
#20703 = CIRCLE ( 'NONE', #11567, 2.649999999999999467 ) ;
#20704 = VERTEX_POINT ( 'NONE', #9109 ) ;
#20705 = AXIS2_PLACEMENT_3D ( 'NONE', #11685, #2148, #3624 ) ;
#20706 = DIRECTION ( 'NONE',  ( 0.000000000000000000, 0.9790840876823220240, 0.2034560130526375243 ) ) ;
#20707 = ORIENTED_EDGE ( 'NONE', *, *, #13067, .F. ) ;
#20708 = LINE ( 'NONE', #12562, #10558 ) ;
#20709 = VECTOR ( 'NONE', #14107, 1000.000000000000000 ) ;
#20710 = ORIENTED_EDGE ( 'NONE', *, *, #14277, .T. ) ;
#20711 = CARTESIAN_POINT ( 'NONE',  ( 6.249999999999902300, -10.82531754730554496, 43.00000000000000000 ) ) ;
#20712 = LINE ( 'NONE', #3029, #20404 ) ;
#20713 = CARTESIAN_POINT ( 'NONE',  ( 14.79893867758297610, -1.779016607511492805E-09, -21.95970808115845685 ) ) ;
#20714 = EDGE_CURVE ( 'NONE', #8788, #6733, #7502, .T. ) ;
#20715 = ORIENTED_EDGE ( 'NONE', *, *, #3539, .T. ) ;
#20716 = DIRECTION ( 'NONE',  ( 0.000000000000000000, 0.000000000000000000, 1.000000000000000000 ) ) ;
#20717 = EDGE_CURVE ( 'NONE', #13680, #1822, #10380, .T. ) ;
#20718 = DIRECTION ( 'NONE',  ( 0.000000000000000000, 0.000000000000000000, 1.000000000000000000 ) ) ;
#20719 = CIRCLE ( 'NONE', #775, 72.00000000007199219 ) ;
#20720 = EDGE_LOOP ( 'NONE', ( #13135, #9675, #9799, #4423, #3570, #9 ) ) ;
#20721 = CARTESIAN_POINT ( 'NONE',  ( 9.580208064738101825, -19.26033094913555388, 77.14905570196101792 ) ) ;
#20722 = CARTESIAN_POINT ( 'NONE',  ( 19.99999999999999645, 0.000000000000000000, 0.000000000000000000 ) ) ;
#20723 = CARTESIAN_POINT ( 'NONE',  ( 0.000000000000000000, 0.000000000000000000, -5.599999999999999645 ) ) ;
#20724 = EDGE_CURVE ( 'NONE', #14260, #19105, #15246, .T. ) ;
#20725 = VERTEX_POINT ( 'NONE', #6031 ) ;
#20726 = DIRECTION ( 'NONE',  ( 1.000000000000000000, 0.000000000000000000, 0.000000000000000000 ) ) ;
#20727 = CARTESIAN_POINT ( 'NONE',  ( 19.99999999999999645, 64.79224928664386596, 2.456263514198732345 ) ) ;
#20728 = VERTEX_POINT ( 'NONE', #9734 ) ;
#20729 = DIRECTION ( 'NONE',  ( 0.000000000000000000, 0.000000000000000000, 1.000000000000000000 ) ) ;
#20730 = AXIS2_PLACEMENT_3D ( 'NONE', #9523, #15992, #1493 ) ;
#20731 = LINE ( 'NONE', #12587, #3104 ) ;
#20732 = AXIS2_PLACEMENT_3D ( 'NONE', #3479, #6456, #5179 ) ;
#20733 = CARTESIAN_POINT ( 'NONE',  ( 10.19618095047497697, -15.25966317163202923, -5.398393749819690335 ) ) ;
#20734 = VECTOR ( 'NONE', #15449, 1000.000000000000000 ) ;
#20735 = ORIENTED_EDGE ( 'NONE', *, *, #10920, .T. ) ;
#20736 = CARTESIAN_POINT ( 'NONE',  ( 0.000000000000000000, 71.89099403602354244, 3.960426305689042970 ) ) ;
#20737 = EDGE_CURVE ( 'NONE', #11443, #15314, #15882, .T. ) ;
#20738 = DIRECTION ( 'NONE',  ( -1.000000000000000000, 0.000000000000000000, -0.000000000000000000 ) ) ;
#20739 = CARTESIAN_POINT ( 'NONE',  ( 40.00000000000000000, -122.3205080756887639, 86.97287527660684248 ) ) ;
#20740 = DIRECTION ( 'NONE',  ( 0.000000000000000000, 0.000000000000000000, 1.000000000000000000 ) ) ;
#20741 = AXIS2_PLACEMENT_3D ( 'NONE', #16191, #17786, #16086 ) ;
#20742 = CARTESIAN_POINT ( 'NONE',  ( -16.62983158437510411, 6.888301784570731279, 9.760112500180310846 ) ) ;
#20743 = EDGE_CURVE ( 'NONE', #1553, #10695, #11118, .T. ) ;
#20744 = EDGE_CURVE ( 'NONE', #2973, #16343, #6340, .T. ) ;
#20745 = CARTESIAN_POINT ( 'NONE',  ( 4.248408729364579806, -6.358192988180021210, -10.73864374981968517 ) ) ;
#20746 = ORIENTED_EDGE ( 'NONE', *, *, #6746, .F. ) ;
#20747 = FACE_OUTER_BOUND ( 'NONE', #5228, .T. ) ;
#20748 = CIRCLE ( 'NONE', #11289, 2.099999999999999645 ) ;
#20749 = CARTESIAN_POINT ( 'NONE',  ( 10.46442989454075168, 10.46442989202483886, 8.944083081519076828 ) ) ;
#20750 = CARTESIAN_POINT ( 'NONE',  ( 85.00002539999999840, 0.000000000000000000, 0.000000000000000000 ) ) ;
#20751 = EDGE_CURVE ( 'NONE', #2701, #5755, #8043, .T. ) ;
#20752 = VERTEX_POINT ( 'NONE', #14412 ) ;
#20753 = DIRECTION ( 'NONE',  ( 0.000000000000000000, 0.000000000000000000, 1.000000000000000000 ) ) ;
#20754 = PLANE ( 'NONE',  #19193 ) ;
#20755 = DIRECTION ( 'NONE',  ( 0.000000000000000000, -0.2697967711570115057, -0.9629172873478027972 ) ) ;
#20756 = AXIS2_PLACEMENT_3D ( 'NONE', #11529, #3373, #14621 ) ;
#20757 = ORIENTED_EDGE ( 'NONE', *, *, #5871, .F. ) ;
#20758 = VECTOR ( 'NONE', #17290, 1000.000000000000000 ) ;
#20759 = DIRECTION ( 'NONE',  ( -0.8660254037844348218, 0.5000000000000066613, 0.000000000000000000 ) ) ;
#20760 = ORIENTED_EDGE ( 'NONE', *, *, #13647, .F. ) ;
#20761 = CARTESIAN_POINT ( 'NONE',  ( -24.99999999999999289, -85.00000000000000000, 8.999999999999984013 ) ) ;
#20762 = CARTESIAN_POINT ( 'NONE',  ( 6.249999999999902300, -10.82531754730554496, 40.00000000000000000 ) ) ;
#20763 = ORIENTED_EDGE ( 'NONE', *, *, #15161, .F. ) ;
#20764 = EDGE_CURVE ( 'NONE', #11513, #8121, #18538, .T. ) ;
#20765 = ORIENTED_EDGE ( 'NONE', *, *, #17541, .T. ) ;
#20766 = DIRECTION ( 'NONE',  ( -1.000000000000000000, 0.000000000000000000, 0.000000000000000000 ) ) ;
#20767 = VECTOR ( 'NONE', #1833, 1000.000000000000000 ) ;
#20768 = CIRCLE ( 'NONE', #14359, 2.649999999999999467 ) ;
#20769 = EDGE_CURVE ( 'NONE', #16945, #14269, #12718, .T. ) ;
#20770 = EDGE_CURVE ( 'NONE', #11465, #19379, #8039, .T. ) ;
#20771 =( REPRESENTATION_RELATIONSHIP ('NONE','NONE', #13739, #3036 ) REPRESENTATION_RELATIONSHIP_WITH_TRANSFORMATION ( #10674 )SHAPE_REPRESENTATION_RELATIONSHIP( ) );
#20772 =( LENGTH_UNIT ( ) NAMED_UNIT ( * ) SI_UNIT ( .MILLI., .METRE. ) );
#20773 = CARTESIAN_POINT ( 'NONE',  ( 5.200000000000002842, 3.061616997868383634E-16, -2.500000000000000444 ) ) ;
#20774 = EDGE_CURVE ( 'NONE', #15895, #13680, #2972, .T. ) ;
#20775 = CARTESIAN_POINT ( 'NONE',  ( 7.575000000000064126, 13.12028486733421850, -40.00000000000000000 ) ) ;
#20776 = CARTESIAN_POINT ( 'NONE',  ( -10.32494394706616703, 4.276731815070943910, -15.90582774935257682 ) ) ;
#20777 = AXIS2_PLACEMENT_3D ( 'NONE', #19626, #19321, #1938 ) ;
#20778 = AXIS2_PLACEMENT_3D ( 'NONE', #17689, #3159, #6842 ) ;
#20779 = CARTESIAN_POINT ( 'NONE',  ( -7.902369976724391343, 7.902369978624323110, 15.26051524971320283 ) ) ;
#20780 = LINE ( 'NONE', #19200, #10200 ) ;
#20781 = VECTOR ( 'NONE', #5509, 1000.000000000000000 ) ;
#20782 = LINE ( 'NONE', #7854, #10791 ) ;
#20783 = LINE ( 'NONE', #1620, #881 ) ;
#20784 = ORIENTED_EDGE ( 'NONE', *, *, #6504, .F. ) ;
#20785 = DIRECTION ( 'NONE',  ( 0.000000000000000000, 0.000000000000000000, 1.000000000000000000 ) ) ;
#20786 = ORIENTED_EDGE ( 'NONE', *, *, #934, .F. ) ;
#20787 = CARTESIAN_POINT ( 'NONE',  ( 10.19618095047497874, -15.25966317163203279, -14.82339374981968483 ) ) ;
#20788 = LINE ( 'NONE', #990, #4889 ) ;
#20789 = ORIENTED_EDGE ( 'NONE', *, *, #7871, .F. ) ;
#20790 = LINE ( 'NONE', #6273, #11305 ) ;
#20791 = ORIENTED_EDGE ( 'NONE', *, *, #7181, .T. ) ;
#20792 = CARTESIAN_POINT ( 'NONE',  ( 3.600000000000060485, 10.82531754730546147, 126.0000000000000000 ) ) ;
#20793 = CARTESIAN_POINT ( 'NONE',  ( 3.600000000000054712, 10.82531754730546147, 40.00000000000000000 ) ) ;
#20794 = DIRECTION ( 'NONE',  ( -0.000000000000000000, -0.000000000000000000, 1.000000000000000000 ) ) ;
#20795 = CIRCLE ( 'NONE', #8262, 35.00000000000000000 ) ;
#20796 = EDGE_LOOP ( 'NONE', ( #13348, #14388, #9167, #14855 ) ) ;
#20797 = DIRECTION ( 'NONE',  ( 0.000000000000000000, 0.1361666490962468723, -0.9906859460363306447 ) ) ;
#20798 = FACE_OUTER_BOUND ( 'NONE', #10576, .T. ) ;
#20799 = DIRECTION ( 'NONE',  ( -0.000000000000000000, -0.000000000000000000, 1.000000000000000000 ) ) ;
#20800 = AXIS2_PLACEMENT_3D ( 'NONE', #1204, #4687, #12430 ) ;
#20801 = CARTESIAN_POINT ( 'NONE',  ( 0.000000000000000000, 0.000000000000000000, 43.00000000000000000 ) ) ;
#20802 = ORIENTED_EDGE ( 'NONE', *, *, #6712, .T. ) ;
#20803 = CARTESIAN_POINT ( 'NONE',  ( 7.500000000000000000, 9.184850993605147944E-16, 40.00000000000000000 ) ) ;
#20804 = LINE ( 'NONE', #12971, #9152 ) ;
#20805 = VERTEX_POINT ( 'NONE', #4747 ) ;
#20806 = AXIS2_PLACEMENT_3D ( 'NONE', #18860, #14407, #17478 ) ;
#20807 = CARTESIAN_POINT ( 'NONE',  ( 1.040949779275250179E-14, -85.00000000000000000, 5.000000000000000000 ) ) ;
#20808 = DIRECTION ( 'NONE',  ( 1.000000000000000000, 0.000000000000000000, 0.000000000000000000 ) ) ;
#20809 = ADVANCED_FACE ( 'NONE', ( #1686 ), #17377, .F. ) ;
#20810 = ORIENTED_EDGE ( 'NONE', *, *, #18575, .F. ) ;
#20811 = ADVANCED_FACE ( 'NONE', ( #20747 ), #7937, .T. ) ;
#20812 = CARTESIAN_POINT ( 'NONE',  ( 2.500000000000000000, -2.357898499370432166, 3.035766082959412415E-15 ) ) ;
#20813 = CARTESIAN_POINT ( 'NONE',  ( -65.00002539999999840, 4.898587196589412829E-16, -4.000000000000000000 ) ) ;
#20814 = CYLINDRICAL_SURFACE ( 'NONE', #9633, 65.24900000006525147 ) ;
#20815 = EDGE_LOOP ( 'NONE', ( #17547, #5106, #15401, #7577 ) ) ;
#20816 = DIRECTION ( 'NONE',  ( 0.000000000000000000, 0.2697967711570183891, 0.9629172873478009098 ) ) ;
#20817 = ORIENTED_EDGE ( 'NONE', *, *, #11069, .T. ) ;
#20818 = CIRCLE ( 'NONE', #15403, 27.60000000002759535 ) ;
#20819 = FACE_OUTER_BOUND ( 'NONE', #6933, .T. ) ;
#20820 = VERTEX_POINT ( 'NONE', #6235 ) ;
#20821 = DIRECTION ( 'NONE',  ( 0.000000000000000000, 0.000000000000000000, 1.000000000000000000 ) ) ;
#20822 = CARTESIAN_POINT ( 'NONE',  ( -52.49999999999999289, -40.00000000000000000, 0.000000000000000000 ) ) ;
#20823 = CARTESIAN_POINT ( 'NONE',  ( 9.999999999999998224, 10.74906464462118016, 71.19310085447973790 ) ) ;
#20824 = CONTEXT_DEPENDENT_SHAPE_REPRESENTATION ( #7366, #13560 ) ;
#20825 = CARTESIAN_POINT ( 'NONE',  ( 2.222972771497741640, 11.17563879704982988, 23.85589100064743207 ) ) ;
#20826 = ORIENTED_EDGE ( 'NONE', *, *, #88, .F. ) ;
#20827 = AXIS2_PLACEMENT_3D ( 'NONE', #8826, #1427, #4703 ) ;
#20828 = FACE_OUTER_BOUND ( 'NONE', #9869, .T. ) ;
#20829 = FACE_BOUND ( 'NONE', #20278, .T. ) ;
#20830 = ORIENTED_EDGE ( 'NONE', *, *, #10670, .F. ) ;
#20831 = CARTESIAN_POINT ( 'NONE',  ( -2.870125743571141808, -6.929096493489625530, -24.95588749981969201 ) ) ;
#20832 = EDGE_CURVE ( 'NONE', #15515, #2965, #13804, .T. ) ;
#20833 = CYLINDRICAL_SURFACE ( 'NONE', #6808, 4.250000000000000000 ) ;
#20834 = DIRECTION ( 'NONE',  ( 0.000000000000000000, 0.000000000000000000, 1.000000000000000000 ) ) ;
#20835 = ORIENTED_EDGE ( 'NONE', *, *, #294, .T. ) ;
#20836 = CIRCLE ( 'NONE', #8649, 27.60000000002760245 ) ;
#20837 = LINE ( 'NONE', #16080, #7345 ) ;
#20838 = CARTESIAN_POINT ( 'NONE',  ( 19.99999999999999645, -58.44960523466261293, 28.06621538408569805 ) ) ;
#20839 = VERTEX_POINT ( 'NONE', #6433 ) ;
#20840 = ADVANCED_FACE ( 'NONE', ( #15984, #1487 ), #2849, .T. ) ;
#20841 = CARTESIAN_POINT ( 'NONE',  ( -22.32752340640299238, -5.629990940594709947, -87.65661170390809787 ) ) ;
#20842 = VECTOR ( 'NONE', #1089, 1000.000000000000000 ) ;
#20843 = CARTESIAN_POINT ( 'NONE',  ( -21.50000000000000000, 0.000000000000000000, -68.00000000000000000 ) ) ;
#20844 = CARTESIAN_POINT ( 'NONE',  ( 15.25966316918061239, -10.19618095414378445, -24.83745624981969513 ) ) ;
#20845 = ORIENTED_EDGE ( 'NONE', *, *, #4835, .T. ) ;
#20846 = CARTESIAN_POINT ( 'NONE',  ( 5.303300858261588147, -5.303300859536636658, -11.03317499981968552 ) ) ;
#20847 = CARTESIAN_POINT ( 'NONE',  ( 19.99999999999999645, 10.77748419466781726, -63.93680186330462334 ) ) ;
#20848 = DIRECTION ( 'NONE',  ( 0.000000000000000000, -1.000000000000000000, 1.471414886128461471E-15 ) ) ;
#20849 = DIRECTION ( 'NONE',  ( 1.000000000000000000, 0.000000000000000000, 0.000000000000000000 ) ) ;
#20850 = CARTESIAN_POINT ( 'NONE',  ( 6.888301780572508193, -16.62983158603122291, -12.62426249981968951 ) ) ;
#20851 = ADVANCED_FACE ( 'NONE', ( #12824 ), #20645, .T. ) ;
#20852 = STYLED_ITEM ( 'NONE', ( #6865 ), #16501 ) ;
#20853 = CARTESIAN_POINT ( 'NONE',  ( 7.500000000000003553, 1.491842754878801580, 9.504268750087788931 ) ) ;
#20854 = CARTESIAN_POINT ( 'NONE',  ( 85.00002539999999840, 0.000000000000000000, 0.000000000000000000 ) ) ;
#20855 = CIRCLE ( 'NONE', #2288, 72.00000000007199219 ) ;
#20856 = AXIS2_PLACEMENT_3D ( 'NONE', #8521, #6936, #10126 ) ;
#20857 = CARTESIAN_POINT ( 'NONE',  ( 13.67243654778934925, 5.663308646854335215, -9.316854418480929212 ) ) ;
#20858 = CARTESIAN_POINT ( 'NONE',  ( 4.000000000000003553, -2.309401076758539784, -5.599999999999999645 ) ) ;
#20859 = ORIENTED_EDGE ( 'NONE', *, *, #18571, .F. ) ;
#20860 = CYLINDRICAL_SURFACE ( 'NONE', #5156, 27.60000000002759535 ) ;
#20861 = DIRECTION ( 'NONE',  ( -1.000000000000000000, -0.000000000000000000, -0.000000000000000000 ) ) ;
#20862 = CARTESIAN_POINT ( 'NONE',  ( 37.34030720104099998, -20.29716165210874479, 71.08834080262353439 ) ) ;
#20863 = ORIENTED_EDGE ( 'NONE', *, *, #12465, .T. ) ;
#20864 = EDGE_CURVE ( 'NONE', #17301, #6711, #17690, .T. ) ;
#20865 = CYLINDRICAL_SURFACE ( 'NONE', #20394, 2.099999999999997868 ) ;
#20866 = CIRCLE ( 'NONE', #11732, 4.000000000000000888 ) ;
#20867 = ORIENTED_EDGE ( 'NONE', *, *, #274, .F. ) ;
#20868 = DIRECTION ( 'NONE',  ( -1.000000000000000000, 0.000000000000000000, -0.000000000000000000 ) ) ;
#20869 = CARTESIAN_POINT ( 'NONE',  ( 7.500000000000000000, 9.184850993605147944E-16, 46.00000000000000711 ) ) ;
#20870 = CIRCLE ( 'NONE', #5296, 65.24900000006525147 ) ;
#20871 = EDGE_CURVE ( 'NONE', #11972, #2396, #19071, .T. ) ;
#20872 = ORIENTED_EDGE ( 'NONE', *, *, #14649, .T. ) ;
#20873 = ORIENTED_EDGE ( 'NONE', *, *, #12572, .F. ) ;
#20874 = CARTESIAN_POINT ( 'NONE',  ( 30.25369199320016023, -108.6370530507956289, -73.18626058406910317 ) ) ;
#20875 = CIRCLE ( 'NONE', #15112, 80.00000000000000000 ) ;
#20876 = MECHANICAL_DESIGN_GEOMETRIC_PRESENTATION_REPRESENTATION (  '', ( #1610 ), #14469 ) ;
#20877 = EDGE_CURVE ( 'NONE', #16643, #15776, #15155, .T. ) ;
#20878 = EDGE_CURVE ( 'NONE', #5163, #12115, #16851, .T. ) ;
#20879 = DIRECTION ( 'NONE',  ( -1.000000000000000000, 0.000000000000000000, -0.000000000000000000 ) ) ;
#20880 = PRODUCT_DEFINITION ( 'UNKNOWN', '', #3877, #8995 ) ;
#20881 = CARTESIAN_POINT ( 'NONE',  ( -11.17563879758428769, -2.222972768810840272, -16.78942149935257788 ) ) ;
#20882 = AXIS2_PLACEMENT_3D ( 'NONE', #2225, #8686, #15159 ) ;
#20883 = CARTESIAN_POINT ( 'NONE',  ( -2.870125741905209971, 6.929096494179676213, -21.42151249981968775 ) ) ;
#20884 = AXIS2_PLACEMENT_3D ( 'NONE', #9305, #17582, #12274 ) ;
#20885 = CYLINDRICAL_SURFACE ( 'NONE', #17658, 11.49999999999999645 ) ;
#20886 = ADVANCED_FACE ( 'NONE', ( #3764 ), #291, .T. ) ;
#20887 = FACE_OUTER_BOUND ( 'NONE', #16373, .T. ) ;
#20888 = CARTESIAN_POINT ( 'NONE',  ( 19.99999999999999645, -63.05226888949902531, 15.11556105343437828 ) ) ;
#20889 = ADVANCED_FACE ( 'NONE', ( #19578 ), #13332, .T. ) ;
#20890 = ORIENTED_EDGE ( 'NONE', *, *, #19573, .F. ) ;
#20891 = CIRCLE ( 'NONE', #18521, 65.24900000006525147 ) ;
#20892 = FACE_OUTER_BOUND ( 'NONE', #16520, .T. ) ;
#20893 = ORIENTED_EDGE ( 'NONE', *, *, #7035, .T. ) ;
#20894 = CARTESIAN_POINT ( 'NONE',  ( 18.00000000043041126, 3.580422610670019434, -7.165581249819687137 ) ) ;
#20895 = DIRECTION ( 'NONE',  ( 1.000000000000000000, -0.000000000000000000, -0.000000000000000000 ) ) ;
#20896 = ORIENTED_EDGE ( 'NONE', *, *, #15226, .F. ) ;
#20897 = CARTESIAN_POINT ( 'NONE',  ( 0.000000000000000000, -39.37110852956777762, -51.51683813304910586 ) ) ;
#20898 = ORIENTED_EDGE ( 'NONE', *, *, #5309, .F. ) ;
#20899 = CARTESIAN_POINT ( 'NONE',  ( 7.500000000000000000, -1.491842755816076060, -8.756668749912215333 ) ) ;
#20900 = DIRECTION ( 'NONE',  ( 0.000000000000000000, 0.000000000000000000, 1.000000000000000000 ) ) ;
#20901 = EDGE_CURVE ( 'NONE', #2530, #8201, #11442, .T. ) ;
#20902 = VERTEX_POINT ( 'NONE', #16395 ) ;
#20903 = DIRECTION ( 'NONE',  ( -1.000000000000000000, 0.000000000000000000, 0.000000000000000000 ) ) ;
#20904 = EDGE_CURVE ( 'NONE', #5132, #4779, #6539, .T. ) ;
#20905 = AXIS2_PLACEMENT_3D ( 'NONE', #3945, #15090, #2052 ) ;
#20906 = FACE_OUTER_BOUND ( 'NONE', #11188, .T. ) ;
#20907 = DIRECTION ( 'NONE',  ( 0.000000000000000000, 0.8169698930104430934, -0.5766803221148656400 ) ) ;
#20908 = CIRCLE ( 'NONE', #3301, 72.00000000007199219 ) ;
#20909 = DIRECTION ( 'NONE',  ( 1.000000000000000000, 0.000000000000000000, 0.000000000000000000 ) ) ;
#20910 = VERTEX_POINT ( 'NONE', #19891 ) ;
#20911 = CARTESIAN_POINT ( 'NONE',  ( -6.232800000000000118, 0.000000000000000000, 10.79377999999999993 ) ) ;
#20912 = CARTESIAN_POINT ( 'NONE',  ( -7.500000000000009770, -1.491842754878800248, 1.631668750087792663 ) ) ;
#20913 = ORIENTED_EDGE ( 'NONE', *, *, #8496, .T. ) ;
#20914 = DIRECTION ( 'NONE',  ( -1.000000000000000000, 0.000000000000000000, 0.000000000000000000 ) ) ;
#20915 = DIRECTION ( 'NONE',  ( -1.000000000000000000, 0.000000000000000000, -0.000000000000000000 ) ) ;
#20916 = ADVANCED_FACE ( 'NONE', ( #3669 ), #11625, .T. ) ;
#20917 = VERTEX_POINT ( 'NONE', #1990 ) ;
#20918 = CARTESIAN_POINT ( 'NONE',  ( 1.084202172485504434E-14, 4.618802153517020059, -5.242734410091827613 ) ) ;
#20919 = CARTESIAN_POINT ( 'NONE',  ( -24.99999999999999289, -85.00000000000000000, -1.040949779275250179E-14 ) ) ;
#20920 = CYLINDRICAL_SURFACE ( 'NONE', #15373, 27.60000000002760245 ) ;
#20921 = EDGE_LOOP ( 'NONE', ( #18471, #3742, #20671, #15065 ) ) ;
#20922 = DIRECTION ( 'NONE',  ( 0.000000000000000000, 0.000000000000000000, -1.000000000000000000 ) ) ;
#20923 = ORIENTED_EDGE ( 'NONE', *, *, #4433, .F. ) ;
#20924 = CYLINDRICAL_SURFACE ( 'NONE', #1758, 72.00000000007199219 ) ;
#20925 = ORIENTED_EDGE ( 'NONE', *, *, #16035, .T. ) ;
#20926 = CARTESIAN_POINT ( 'NONE',  ( 30.00000000000000355, -139.6410161513775563, -90.00000000000001421 ) ) ;
#20927 = ADVANCED_FACE ( 'NONE', ( #5365, #9824, #10042, #391, #11430, #14714 ), #6741, .T. ) ;
#20928 = DIRECTION ( 'NONE',  ( -1.000000000000000000, 0.000000000000000000, 0.000000000000000000 ) ) ;
#20929 = CARTESIAN_POINT ( 'NONE',  ( 4.276731815070943910, 10.32494394706616703, 24.15042225064743420 ) ) ;
#20930 = ORIENTED_EDGE ( 'NONE', *, *, #5309, .T. ) ;
#20931 = CARTESIAN_POINT ( 'NONE',  ( 7.500000000000004441, -8.788009009181406898E-15, -18.47619999999769647 ) ) ;
#20932 = DIRECTION ( 'NONE',  ( -0.000000000000000000, 0.000000000000000000, 1.000000000000000000 ) ) ;
#20933 = VERTEX_POINT ( 'NONE', #16595 ) ;
#20934 = DIRECTION ( 'NONE',  ( 0.000000000000000000, -0.7308359642781301346, 0.6825531432186475733 ) ) ;
#20935 = CARTESIAN_POINT ( 'NONE',  ( -6.888301780572501976, 16.62983158603122291, 20.36323750018031475 ) ) ;
#20936 = LINE ( 'NONE', #17060, #10398 ) ;
#20937 = DIRECTION ( 'NONE',  ( 0.000000000000000000, 0.000000000000000000, 1.000000000000000000 ) ) ;
#20938 = ORIENTED_EDGE ( 'NONE', *, *, #3374, .F. ) ;
#20939 = DIRECTION ( 'NONE',  ( -0.000000000000000000, -0.000000000000000000, 1.000000000000000000 ) ) ;
#20940 = FACE_BOUND ( 'NONE', #4393, .T. ) ;
#20941 = ORIENTED_EDGE ( 'NONE', *, *, #5451, .F. ) ;
#20942 = CYLINDRICAL_SURFACE ( 'NONE', #11261, 65.24900000006525147 ) ;
#20943 = DIRECTION ( 'NONE',  ( 0.000000000000000000, -0.9790840876823249106, 0.2034560130526240629 ) ) ;
#20944 = NEXT_ASSEMBLY_USAGE_OCCURRENCE ( 'NAUO1', ' ', ' ', #10520, #20880, $ ) ;
#20945 = NEXT_ASSEMBLY_USAGE_OCCURRENCE ( 'NAUO2', ' ', ' ', #10520, #2358, $ ) ;
#20946 = NEXT_ASSEMBLY_USAGE_OCCURRENCE ( 'NAUO3', ' ', ' ', #10520, #17526, $ ) ;
#20947 = NEXT_ASSEMBLY_USAGE_OCCURRENCE ( 'NAUO4', ' ', ' ', #10520, #17783, $ ) ;
#20948 = NEXT_ASSEMBLY_USAGE_OCCURRENCE ( 'NAUO5', ' ', ' ', #10520, #15563, $ ) ;
#20949 = NEXT_ASSEMBLY_USAGE_OCCURRENCE ( 'NAUO6', ' ', ' ', #10520, #13380, $ ) ;
#20950 = NEXT_ASSEMBLY_USAGE_OCCURRENCE ( 'NAUO7', ' ', ' ', #10520, #13380, $ ) ;
#20951 = NEXT_ASSEMBLY_USAGE_OCCURRENCE ( 'NAUO8', ' ', ' ', #10520, #13380, $ ) ;
#20952 = NEXT_ASSEMBLY_USAGE_OCCURRENCE ( 'NAUO9', ' ', ' ', #10520, #4023, $ ) ;
#20953 = NEXT_ASSEMBLY_USAGE_OCCURRENCE ( 'NAUO10', ' ', ' ', #10520, #13380, $ ) ;
#20954 = NEXT_ASSEMBLY_USAGE_OCCURRENCE ( 'NAUO11', ' ', ' ', #10520, #19582, $ ) ;
#20955 = NEXT_ASSEMBLY_USAGE_OCCURRENCE ( 'NAUO12', ' ', ' ', #10520, #19582, $ ) ;
#20956 = NEXT_ASSEMBLY_USAGE_OCCURRENCE ( 'NAUO13', ' ', ' ', #10520, #19582, $ ) ;
#20957 = NEXT_ASSEMBLY_USAGE_OCCURRENCE ( 'NAUO14', ' ', ' ', #10520, #19582, $ ) ;
#20958 = NEXT_ASSEMBLY_USAGE_OCCURRENCE ( 'NAUO15', ' ', ' ', #10520, #15841, $ ) ;
#20959 = NEXT_ASSEMBLY_USAGE_OCCURRENCE ( 'NAUO16', ' ', ' ', #10520, #17130, $ ) ;
#20960 = NEXT_ASSEMBLY_USAGE_OCCURRENCE ( 'NAUO17', ' ', ' ', #10520, #17130, $ ) ;
#20961 = NEXT_ASSEMBLY_USAGE_OCCURRENCE ( 'NAUO18', ' ', ' ', #10520, #17130, $ ) ;
#20962 = NEXT_ASSEMBLY_USAGE_OCCURRENCE ( 'NAUO19', ' ', ' ', #10520, #15841, $ ) ;
#20963 = NEXT_ASSEMBLY_USAGE_OCCURRENCE ( 'NAUO20', ' ', ' ', #10520, #15841, $ ) ;
#20964 = NEXT_ASSEMBLY_USAGE_OCCURRENCE ( 'NAUO21', ' ', ' ', #10520, #17130, $ ) ;
#20965 = NEXT_ASSEMBLY_USAGE_OCCURRENCE ( 'NAUO22', ' ', ' ', #10520, #15841, $ ) ;
#20966 = NEXT_ASSEMBLY_USAGE_OCCURRENCE ( 'NAUO23', ' ', ' ', #10520, #17130, $ ) ;
#20967 = NEXT_ASSEMBLY_USAGE_OCCURRENCE ( 'NAUO24', ' ', ' ', #10520, #17130, $ ) ;
#20968 = NEXT_ASSEMBLY_USAGE_OCCURRENCE ( 'NAUO25', ' ', ' ', #10520, #15841, $ ) ;
#20969 = NEXT_ASSEMBLY_USAGE_OCCURRENCE ( 'NAUO26', ' ', ' ', #10520, #15841, $ ) ;
ENDSEC;
END-ISO-10303-21;
